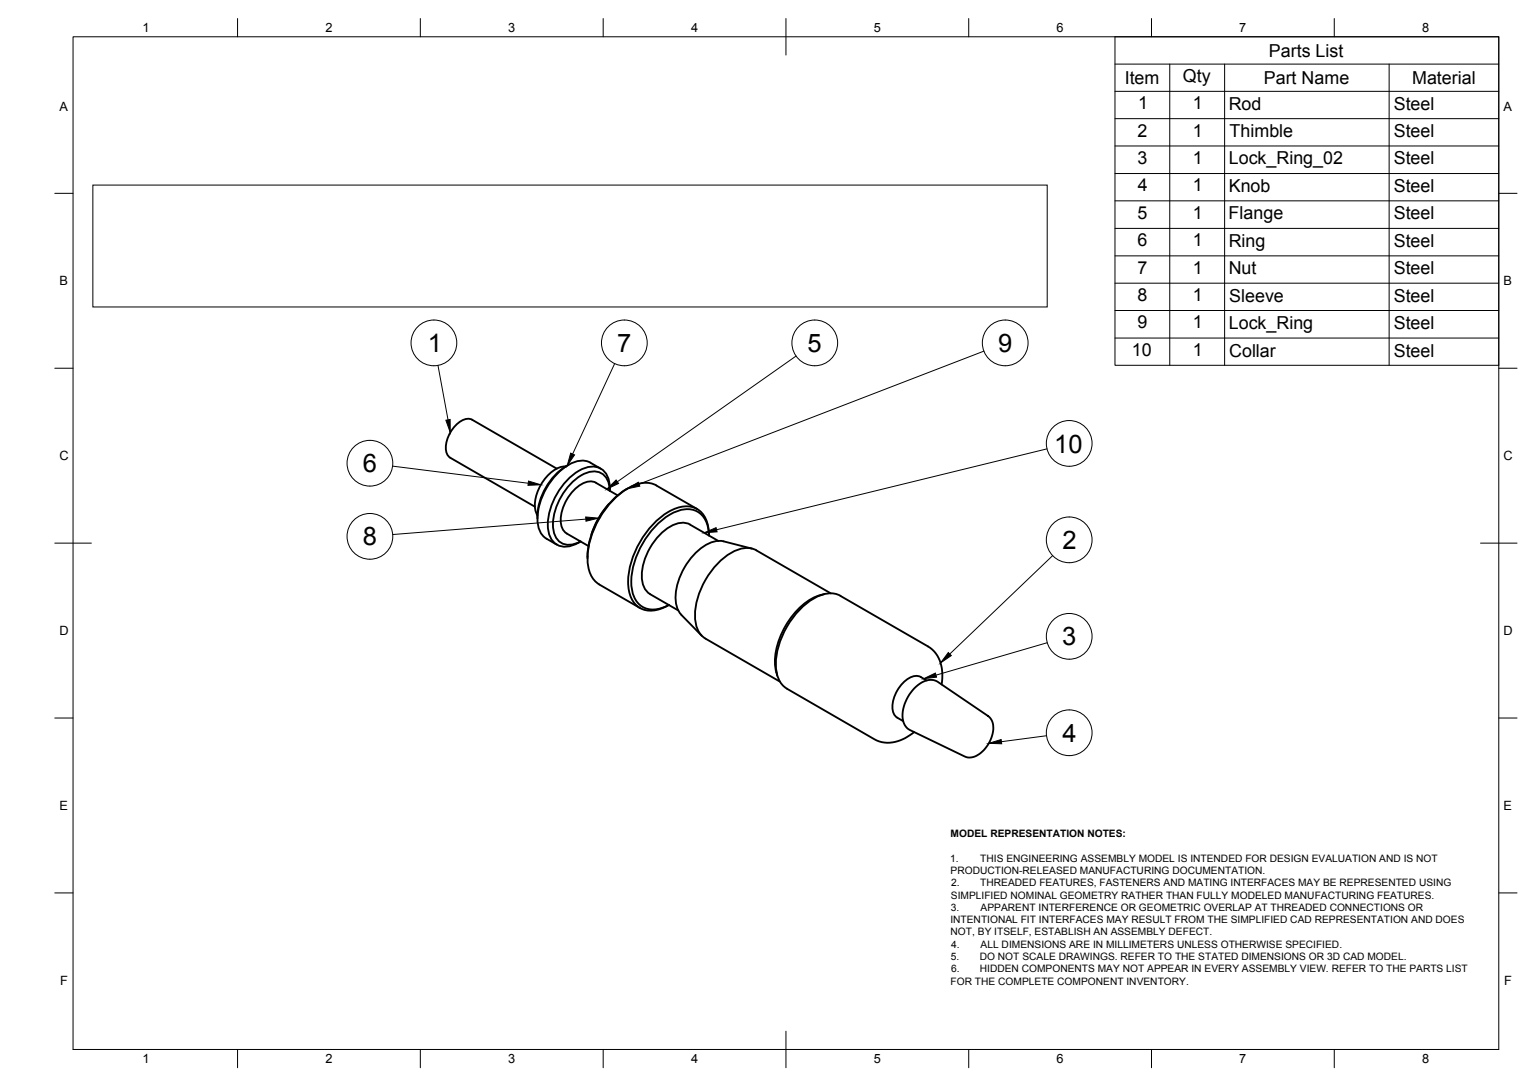
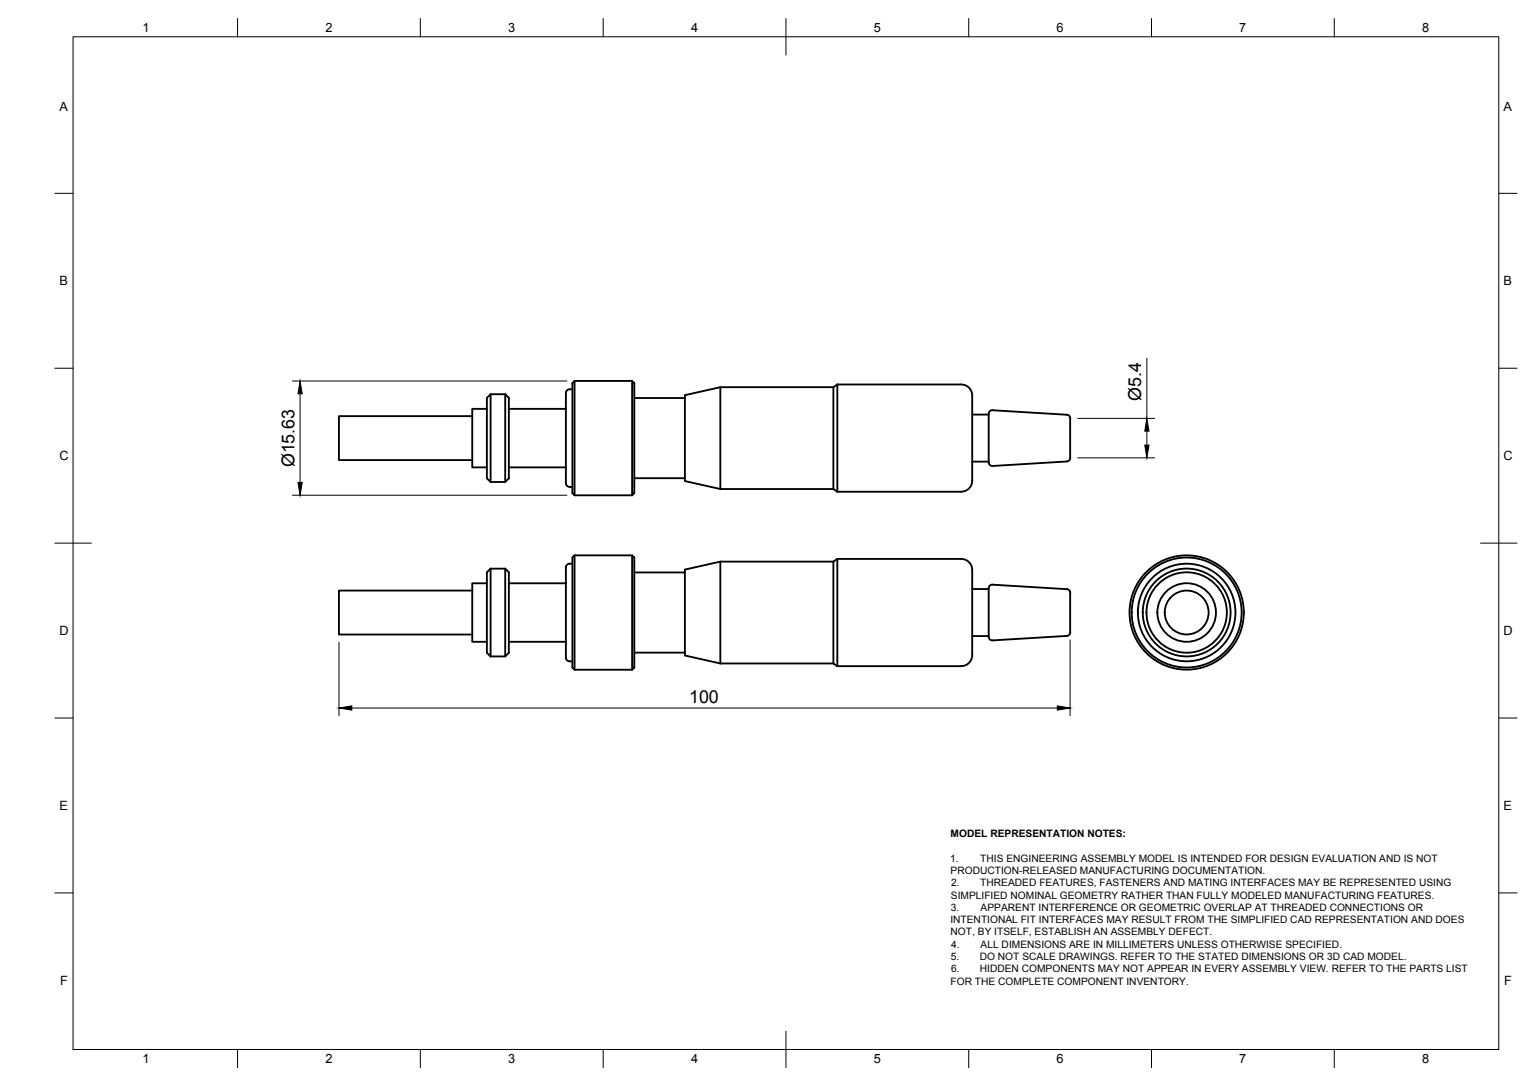
ISO-10303-21;
HEADER;
/* Generated by software containing ST-Developer
 * from STEP Tools, Inc. (www.steptools.com) 
 */

FILE_DESCRIPTION(
/* description */ (''),
/* implementation_level */ '2;1');

FILE_NAME(
/* name */ 'BR-156',
/* time_stamp */ '2026-10-05T01:33:24-07:00',
/* author */ (''),
/* organization */ (''),
/* preprocessor_version */ 'ST-DEVELOPER v20.2',
/* originating_system */ 'Autodesk Translation Framework v15.15.0.0',
/* authorisation */ '');

FILE_SCHEMA (('AUTOMOTIVE_DESIGN { 1 0 10303 214 3 1 1 }'));
ENDSEC;

DATA;
#10=MECHANICAL_DESIGN_GEOMETRIC_PRESENTATION_REPRESENTATION('',(#82,#83,
#84,#85,#86,#87,#88,#89,#90,#91),#1128);
#11=ITEM_DEFINED_TRANSFORMATION($,$,#643,#731);
#12=ITEM_DEFINED_TRANSFORMATION($,$,#649,#732);
#13=ITEM_DEFINED_TRANSFORMATION($,$,#664,#733);
#14=ITEM_DEFINED_TRANSFORMATION($,$,#670,#734);
#15=ITEM_DEFINED_TRANSFORMATION($,$,#682,#735);
#16=ITEM_DEFINED_TRANSFORMATION($,$,#688,#736);
#17=ITEM_DEFINED_TRANSFORMATION($,$,#694,#737);
#18=ITEM_DEFINED_TRANSFORMATION($,$,#704,#738);
#19=ITEM_DEFINED_TRANSFORMATION($,$,#713,#739);
#20=ITEM_DEFINED_TRANSFORMATION($,$,#725,#740);
#21=(
REPRESENTATION_RELATIONSHIP($,$,#1166,#1165)
REPRESENTATION_RELATIONSHIP_WITH_TRANSFORMATION(#11)
SHAPE_REPRESENTATION_RELATIONSHIP()
);
#22=(
REPRESENTATION_RELATIONSHIP($,$,#1167,#1165)
REPRESENTATION_RELATIONSHIP_WITH_TRANSFORMATION(#12)
SHAPE_REPRESENTATION_RELATIONSHIP()
);
#23=(
REPRESENTATION_RELATIONSHIP($,$,#1168,#1165)
REPRESENTATION_RELATIONSHIP_WITH_TRANSFORMATION(#13)
SHAPE_REPRESENTATION_RELATIONSHIP()
);
#24=(
REPRESENTATION_RELATIONSHIP($,$,#1169,#1165)
REPRESENTATION_RELATIONSHIP_WITH_TRANSFORMATION(#14)
SHAPE_REPRESENTATION_RELATIONSHIP()
);
#25=(
REPRESENTATION_RELATIONSHIP($,$,#1170,#1165)
REPRESENTATION_RELATIONSHIP_WITH_TRANSFORMATION(#15)
SHAPE_REPRESENTATION_RELATIONSHIP()
);
#26=(
REPRESENTATION_RELATIONSHIP($,$,#1171,#1165)
REPRESENTATION_RELATIONSHIP_WITH_TRANSFORMATION(#16)
SHAPE_REPRESENTATION_RELATIONSHIP()
);
#27=(
REPRESENTATION_RELATIONSHIP($,$,#1172,#1165)
REPRESENTATION_RELATIONSHIP_WITH_TRANSFORMATION(#17)
SHAPE_REPRESENTATION_RELATIONSHIP()
);
#28=(
REPRESENTATION_RELATIONSHIP($,$,#1173,#1165)
REPRESENTATION_RELATIONSHIP_WITH_TRANSFORMATION(#18)
SHAPE_REPRESENTATION_RELATIONSHIP()
);
#29=(
REPRESENTATION_RELATIONSHIP($,$,#1174,#1165)
REPRESENTATION_RELATIONSHIP_WITH_TRANSFORMATION(#19)
SHAPE_REPRESENTATION_RELATIONSHIP()
);
#30=(
REPRESENTATION_RELATIONSHIP($,$,#1175,#1165)
REPRESENTATION_RELATIONSHIP_WITH_TRANSFORMATION(#20)
SHAPE_REPRESENTATION_RELATIONSHIP()
);
#31=CONTEXT_DEPENDENT_SHAPE_REPRESENTATION(#21,#1155);
#32=CONTEXT_DEPENDENT_SHAPE_REPRESENTATION(#22,#1156);
#33=CONTEXT_DEPENDENT_SHAPE_REPRESENTATION(#23,#1157);
#34=CONTEXT_DEPENDENT_SHAPE_REPRESENTATION(#24,#1158);
#35=CONTEXT_DEPENDENT_SHAPE_REPRESENTATION(#25,#1159);
#36=CONTEXT_DEPENDENT_SHAPE_REPRESENTATION(#26,#1160);
#37=CONTEXT_DEPENDENT_SHAPE_REPRESENTATION(#27,#1161);
#38=CONTEXT_DEPENDENT_SHAPE_REPRESENTATION(#28,#1162);
#39=CONTEXT_DEPENDENT_SHAPE_REPRESENTATION(#29,#1163);
#40=CONTEXT_DEPENDENT_SHAPE_REPRESENTATION(#30,#1164);
#41=NEXT_ASSEMBLY_USAGE_OCCURRENCE('Rod:1','Rod:1','Rod:1',#1177,#1178,
'Rod:1');
#42=NEXT_ASSEMBLY_USAGE_OCCURRENCE('Thimble:1','Thimble:1','Thimble:1',
#1177,#1179,'Thimble:1');
#43=NEXT_ASSEMBLY_USAGE_OCCURRENCE('Lock_Ring_02:1','Lock_Ring_02:1',
'Lock_Ring_02:1',#1177,#1180,'Lock_Ring_02:1');
#44=NEXT_ASSEMBLY_USAGE_OCCURRENCE('Knob:1','Knob:1','Knob:1',#1177,#1181,
'Knob:1');
#45=NEXT_ASSEMBLY_USAGE_OCCURRENCE('Flange:1','Flange:1','Flange:1',#1177,
#1182,'Flange:1');
#46=NEXT_ASSEMBLY_USAGE_OCCURRENCE('Ring:1','Ring:1','Ring:1',#1177,#1183,
'Ring:1');
#47=NEXT_ASSEMBLY_USAGE_OCCURRENCE('Nut:1','Nut:1','Nut:1',#1177,#1184,
'Nut:1');
#48=NEXT_ASSEMBLY_USAGE_OCCURRENCE('Sleeve:1','Sleeve:1','Sleeve:1',#1177,
#1185,'Sleeve:1');
#49=NEXT_ASSEMBLY_USAGE_OCCURRENCE('Lock_Ring:1','Lock_Ring:1',
'Lock_Ring:1',#1177,#1186,'Lock_Ring:1');
#50=NEXT_ASSEMBLY_USAGE_OCCURRENCE('Collar:1','Collar:1','Collar:1',#1177,
#1187,'Collar:1');
#51=TOROIDAL_SURFACE('',#659,5.82799886529799,1.5);
#52=TOROIDAL_SURFACE('',#673,3.3075988470339,0.49999999999999);
#53=TOROIDAL_SURFACE('',#678,2.69979677377649,0.500000000000025);
#54=TOROIDAL_SURFACE('',#709,6.1693331034204,0.499999999999997);
#55=CONICAL_SURFACE('',#650,6.41661225190487,0.22222982204112);
#56=CONICAL_SURFACE('',#655,7.14605510547863,0.59398290857058);
#57=CONICAL_SURFACE('',#676,3.50280261490539,0.0598485673150425);
#58=CONICAL_SURFACE('',#695,5.75,0.785398163397451);
#59=CONICAL_SURFACE('',#700,5.75,0.785398163397451);
#60=CONICAL_SURFACE('',#714,7.66499874644978,0.785398163397445);
#61=CONICAL_SURFACE('',#722,7.66499874644978,0.785398163397452);
#62=SHAPE_REPRESENTATION_RELATIONSHIP('SRR','None',#1166,#72);
#63=SHAPE_REPRESENTATION_RELATIONSHIP('SRR','None',#1167,#73);
#64=SHAPE_REPRESENTATION_RELATIONSHIP('SRR','None',#1168,#74);
#65=SHAPE_REPRESENTATION_RELATIONSHIP('SRR','None',#1169,#75);
#66=SHAPE_REPRESENTATION_RELATIONSHIP('SRR','None',#1170,#76);
#67=SHAPE_REPRESENTATION_RELATIONSHIP('SRR','None',#1171,#77);
#68=SHAPE_REPRESENTATION_RELATIONSHIP('SRR','None',#1172,#78);
#69=SHAPE_REPRESENTATION_RELATIONSHIP('SRR','None',#1173,#79);
#70=SHAPE_REPRESENTATION_RELATIONSHIP('SRR','None',#1174,#80);
#71=SHAPE_REPRESENTATION_RELATIONSHIP('SRR','None',#1175,#81);
#72=ADVANCED_BREP_SHAPE_REPRESENTATION('',(#92),#1118);
#73=ADVANCED_BREP_SHAPE_REPRESENTATION('',(#93),#1119);
#74=ADVANCED_BREP_SHAPE_REPRESENTATION('',(#94),#1120);
#75=ADVANCED_BREP_SHAPE_REPRESENTATION('',(#95),#1121);
#76=ADVANCED_BREP_SHAPE_REPRESENTATION('',(#96),#1122);
#77=ADVANCED_BREP_SHAPE_REPRESENTATION('',(#97),#1123);
#78=ADVANCED_BREP_SHAPE_REPRESENTATION('',(#98),#1124);
#79=ADVANCED_BREP_SHAPE_REPRESENTATION('',(#99),#1125);
#80=ADVANCED_BREP_SHAPE_REPRESENTATION('',(#100),#1126);
#81=ADVANCED_BREP_SHAPE_REPRESENTATION('',(#101),#1127);
#82=STYLED_ITEM('',(#1225),#92);
#83=STYLED_ITEM('',(#1225),#93);
#84=STYLED_ITEM('',(#1226),#94);
#85=STYLED_ITEM('',(#1225),#95);
#86=STYLED_ITEM('',(#1227),#96);
#87=STYLED_ITEM('',(#1227),#97);
#88=STYLED_ITEM('',(#1227),#98);
#89=STYLED_ITEM('',(#1227),#99);
#90=STYLED_ITEM('',(#1225),#100);
#91=STYLED_ITEM('',(#1225),#101);
#92=MANIFOLD_SOLID_BREP('Body1',#521);
#93=MANIFOLD_SOLID_BREP('Body1',#522);
#94=MANIFOLD_SOLID_BREP('Body1',#523);
#95=MANIFOLD_SOLID_BREP('Body1',#524);
#96=MANIFOLD_SOLID_BREP('Body1',#525);
#97=MANIFOLD_SOLID_BREP('Body1',#526);
#98=MANIFOLD_SOLID_BREP('Body1',#527);
#99=MANIFOLD_SOLID_BREP('Body1',#528);
#100=MANIFOLD_SOLID_BREP('Body1',#529);
#101=MANIFOLD_SOLID_BREP('Body1',#530);
#102=LINE('',#964,#119);
#103=LINE('',#971,#120);
#104=LINE('',#976,#121);
#105=LINE('',#980,#122);
#106=LINE('',#984,#123);
#107=LINE('',#996,#124);
#108=LINE('',#1010,#125);
#109=LINE('',#1025,#126);
#110=LINE('',#1034,#127);
#111=LINE('',#1040,#128);
#112=LINE('',#1045,#129);
#113=LINE('',#1048,#130);
#114=LINE('',#1064,#131);
#115=LINE('',#1071,#132);
#116=LINE('',#1076,#133);
#117=LINE('',#1083,#134);
#118=LINE('',#1094,#135);
#119=VECTOR('',#753,3.);
#120=VECTOR('',#762,6.41661225190487);
#121=VECTOR('',#769,6.96411134565927);
#122=VECTOR('',#774,7.14605510547863);
#123=VECTOR('',#779,7.327998865298);
#124=VECTOR('',#796,3.21047290937838);
#125=VECTOR('',#817,3.50280261490539);
#126=VECTOR('',#840,4.);
#127=VECTOR('',#853,4.);
#128=VECTOR('',#860,5.75);
#129=VECTOR('',#867,6.);
#130=VECTOR('',#870,5.75);
#131=VECTOR('',#895,6.66933310342039);
#132=VECTOR('',#902,7.66499874644978);
#133=VECTOR('',#909,7.81499874644978);
#134=VECTOR('',#918,7.66499874644978);
#135=VECTOR('',#935,5.48257260644808);
#136=CYLINDRICAL_SURFACE('',#646,3.);
#137=CYLINDRICAL_SURFACE('',#653,6.96411134565927);
#138=CYLINDRICAL_SURFACE('',#657,7.327998865298);
#139=CYLINDRICAL_SURFACE('',#665,3.21047290937838);
#140=CYLINDRICAL_SURFACE('',#687,4.);
#141=CYLINDRICAL_SURFACE('',#693,4.);
#142=CYLINDRICAL_SURFACE('',#698,6.);
#143=CYLINDRICAL_SURFACE('',#712,6.66933310342039);
#144=CYLINDRICAL_SURFACE('',#718,7.81499874644978);
#145=CYLINDRICAL_SURFACE('',#730,5.48257260644808);
#146=FACE_OUTER_BOUND('',#187,.T.);
#147=FACE_OUTER_BOUND('',#188,.T.);
#148=FACE_OUTER_BOUND('',#189,.T.);
#149=FACE_OUTER_BOUND('',#190,.T.);
#150=FACE_OUTER_BOUND('',#191,.T.);
#151=FACE_OUTER_BOUND('',#192,.T.);
#152=FACE_OUTER_BOUND('',#193,.T.);
#153=FACE_OUTER_BOUND('',#194,.T.);
#154=FACE_OUTER_BOUND('',#195,.T.);
#155=FACE_OUTER_BOUND('',#196,.T.);
#156=FACE_OUTER_BOUND('',#197,.T.);
#157=FACE_OUTER_BOUND('',#198,.T.);
#158=FACE_OUTER_BOUND('',#199,.T.);
#159=FACE_OUTER_BOUND('',#200,.T.);
#160=FACE_OUTER_BOUND('',#201,.T.);
#161=FACE_OUTER_BOUND('',#202,.T.);
#162=FACE_OUTER_BOUND('',#203,.T.);
#163=FACE_OUTER_BOUND('',#204,.T.);
#164=FACE_OUTER_BOUND('',#205,.T.);
#165=FACE_OUTER_BOUND('',#206,.T.);
#166=FACE_OUTER_BOUND('',#207,.T.);
#167=FACE_OUTER_BOUND('',#208,.T.);
#168=FACE_OUTER_BOUND('',#209,.T.);
#169=FACE_OUTER_BOUND('',#210,.T.);
#170=FACE_OUTER_BOUND('',#211,.T.);
#171=FACE_OUTER_BOUND('',#212,.T.);
#172=FACE_OUTER_BOUND('',#213,.T.);
#173=FACE_OUTER_BOUND('',#214,.T.);
#174=FACE_OUTER_BOUND('',#215,.T.);
#175=FACE_OUTER_BOUND('',#216,.T.);
#176=FACE_OUTER_BOUND('',#217,.T.);
#177=FACE_OUTER_BOUND('',#218,.T.);
#178=FACE_OUTER_BOUND('',#219,.T.);
#179=FACE_OUTER_BOUND('',#220,.T.);
#180=FACE_OUTER_BOUND('',#221,.T.);
#181=FACE_OUTER_BOUND('',#222,.T.);
#182=FACE_OUTER_BOUND('',#223,.T.);
#183=FACE_OUTER_BOUND('',#224,.T.);
#184=FACE_OUTER_BOUND('',#225,.T.);
#185=FACE_OUTER_BOUND('',#226,.T.);
#186=FACE_OUTER_BOUND('',#227,.T.);
#187=EDGE_LOOP('',(#352));
#188=EDGE_LOOP('',(#353,#354,#355,#356));
#189=EDGE_LOOP('',(#357));
#190=EDGE_LOOP('',(#358,#359,#360,#361));
#191=EDGE_LOOP('',(#362,#363,#364,#365));
#192=EDGE_LOOP('',(#366,#367,#368,#369));
#193=EDGE_LOOP('',(#370,#371,#372,#373));
#194=EDGE_LOOP('',(#374,#375,#376,#377));
#195=EDGE_LOOP('',(#378));
#196=EDGE_LOOP('',(#379));
#197=EDGE_LOOP('',(#380,#381,#382,#383));
#198=EDGE_LOOP('',(#384));
#199=EDGE_LOOP('',(#385));
#200=EDGE_LOOP('',(#386));
#201=EDGE_LOOP('',(#387,#388,#389,#390));
#202=EDGE_LOOP('',(#391,#392,#393,#394));
#203=EDGE_LOOP('',(#395,#396,#397,#398));
#204=EDGE_LOOP('',(#399));
#205=EDGE_LOOP('',(#400));
#206=EDGE_LOOP('',(#401));
#207=EDGE_LOOP('',(#402,#403,#404,#405));
#208=EDGE_LOOP('',(#406));
#209=EDGE_LOOP('',(#407));
#210=EDGE_LOOP('',(#408,#409,#410,#411));
#211=EDGE_LOOP('',(#412,#413,#414,#415));
#212=EDGE_LOOP('',(#416,#417,#418,#419));
#213=EDGE_LOOP('',(#420,#421,#422,#423));
#214=EDGE_LOOP('',(#424));
#215=EDGE_LOOP('',(#425));
#216=EDGE_LOOP('',(#426));
#217=EDGE_LOOP('',(#427));
#218=EDGE_LOOP('',(#428,#429,#430,#431));
#219=EDGE_LOOP('',(#432,#433,#434,#435));
#220=EDGE_LOOP('',(#436,#437,#438,#439,#440));
#221=EDGE_LOOP('',(#441,#442,#443,#444,#445,#446));
#222=EDGE_LOOP('',(#447));
#223=EDGE_LOOP('',(#448,#449,#450,#451,#452));
#224=EDGE_LOOP('',(#453));
#225=EDGE_LOOP('',(#454));
#226=EDGE_LOOP('',(#455));
#227=EDGE_LOOP('',(#456,#457,#458,#459));
#228=CIRCLE('',#645,3.);
#229=CIRCLE('',#647,3.);
#230=CIRCLE('',#651,6.96411134565927);
#231=CIRCLE('',#652,5.86911315815046);
#232=CIRCLE('',#654,6.96411134565926);
#233=CIRCLE('',#656,7.327998865298);
#234=CIRCLE('',#658,7.327998865298);
#235=CIRCLE('',#660,5.827998865298);
#236=CIRCLE('',#661,1.5);
#237=CIRCLE('',#666,3.21047290937838);
#238=CIRCLE('',#667,3.21047290937838);
#239=CIRCLE('',#672,3.3075988470339);
#240=CIRCLE('',#674,3.80670365153407);
#241=CIRCLE('',#675,0.49999999999999);
#242=CIRCLE('',#677,3.1989015782767);
#243=CIRCLE('',#679,2.69979677377651);
#244=CIRCLE('',#680,0.500000000000025);
#245=CIRCLE('',#684,4.);
#246=CIRCLE('',#686,4.);
#247=CIRCLE('',#690,4.);
#248=CIRCLE('',#692,4.);
#249=CIRCLE('',#696,6.);
#250=CIRCLE('',#697,5.5);
#251=CIRCLE('',#699,6.);
#252=CIRCLE('',#701,5.5);
#253=CIRCLE('',#706,6.66933310342039);
#254=CIRCLE('',#708,6.16933310342039);
#255=CIRCLE('',#710,6.66933310342039);
#256=CIRCLE('',#711,0.499999999999997);
#257=CIRCLE('',#715,7.81499874644978);
#258=CIRCLE('',#716,7.51499874644978);
#259=CIRCLE('',#717,7.81499874644978);
#260=CIRCLE('',#719,7.81499874644978);
#261=CIRCLE('',#720,7.81499874644978);
#262=CIRCLE('',#723,7.51499874644978);
#263=CIRCLE('',#727,5.48257260644808);
#264=CIRCLE('',#729,5.48257260644808);
#265=VERTEX_POINT('',#959);
#266=VERTEX_POINT('',#962);
#267=VERTEX_POINT('',#968);
#268=VERTEX_POINT('',#970);
#269=VERTEX_POINT('',#974);
#270=VERTEX_POINT('',#978);
#271=VERTEX_POINT('',#982);
#272=VERTEX_POINT('',#986);
#273=VERTEX_POINT('',#993);
#274=VERTEX_POINT('',#995);
#275=VERTEX_POINT('',#1002);
#276=VERTEX_POINT('',#1005);
#277=VERTEX_POINT('',#1009);
#278=VERTEX_POINT('',#1013);
#279=VERTEX_POINT('',#1019);
#280=VERTEX_POINT('',#1022);
#281=VERTEX_POINT('',#1028);
#282=VERTEX_POINT('',#1031);
#283=VERTEX_POINT('',#1037);
#284=VERTEX_POINT('',#1039);
#285=VERTEX_POINT('',#1043);
#286=VERTEX_POINT('',#1047);
#287=VERTEX_POINT('',#1054);
#288=VERTEX_POINT('',#1057);
#289=VERTEX_POINT('',#1060);
#290=VERTEX_POINT('',#1067);
#291=VERTEX_POINT('',#1068);
#292=VERTEX_POINT('',#1070);
#293=VERTEX_POINT('',#1075);
#294=VERTEX_POINT('',#1077);
#295=VERTEX_POINT('',#1082);
#296=VERTEX_POINT('',#1088);
#297=VERTEX_POINT('',#1091);
#298=EDGE_CURVE('',#265,#265,#228,.T.);
#299=EDGE_CURVE('',#266,#266,#229,.T.);
#300=EDGE_CURVE('',#266,#265,#102,.T.);
#301=EDGE_CURVE('',#267,#267,#230,.T.);
#302=EDGE_CURVE('',#267,#268,#103,.T.);
#303=EDGE_CURVE('',#268,#268,#231,.T.);
#304=EDGE_CURVE('',#269,#269,#232,.T.);
#305=EDGE_CURVE('',#269,#267,#104,.T.);
#306=EDGE_CURVE('',#270,#270,#233,.T.);
#307=EDGE_CURVE('',#270,#269,#105,.T.);
#308=EDGE_CURVE('',#271,#271,#234,.T.);
#309=EDGE_CURVE('',#271,#270,#106,.T.);
#310=EDGE_CURVE('',#272,#272,#235,.T.);
#311=EDGE_CURVE('',#272,#271,#236,.T.);
#312=EDGE_CURVE('',#273,#273,#237,.T.);
#313=EDGE_CURVE('',#273,#274,#107,.T.);
#314=EDGE_CURVE('',#274,#274,#238,.T.);
#315=EDGE_CURVE('',#275,#275,#239,.T.);
#316=EDGE_CURVE('',#276,#276,#240,.T.);
#317=EDGE_CURVE('',#276,#275,#241,.T.);
#318=EDGE_CURVE('',#276,#277,#108,.T.);
#319=EDGE_CURVE('',#277,#277,#242,.T.);
#320=EDGE_CURVE('',#278,#278,#243,.T.);
#321=EDGE_CURVE('',#278,#277,#244,.T.);
#322=EDGE_CURVE('',#279,#279,#245,.T.);
#323=EDGE_CURVE('',#280,#280,#246,.T.);
#324=EDGE_CURVE('',#279,#280,#109,.T.);
#325=EDGE_CURVE('',#281,#281,#247,.T.);
#326=EDGE_CURVE('',#282,#282,#248,.T.);
#327=EDGE_CURVE('',#281,#282,#110,.T.);
#328=EDGE_CURVE('',#283,#283,#249,.T.);
#329=EDGE_CURVE('',#283,#284,#111,.T.);
#330=EDGE_CURVE('',#284,#284,#250,.T.);
#331=EDGE_CURVE('',#285,#285,#251,.T.);
#332=EDGE_CURVE('',#285,#283,#112,.T.);
#333=EDGE_CURVE('',#285,#286,#113,.T.);
#334=EDGE_CURVE('',#286,#286,#252,.T.);
#335=EDGE_CURVE('',#287,#287,#253,.T.);
#336=EDGE_CURVE('',#288,#288,#254,.T.);
#337=EDGE_CURVE('',#289,#289,#255,.T.);
#338=EDGE_CURVE('',#289,#288,#256,.T.);
#339=EDGE_CURVE('',#287,#289,#114,.T.);
#340=EDGE_CURVE('',#290,#291,#257,.T.);
#341=EDGE_CURVE('',#291,#292,#115,.T.);
#342=EDGE_CURVE('',#292,#292,#258,.T.);
#343=EDGE_CURVE('',#291,#290,#259,.T.);
#344=EDGE_CURVE('',#290,#293,#116,.T.);
#345=EDGE_CURVE('',#294,#293,#260,.T.);
#346=EDGE_CURVE('',#293,#294,#261,.T.);
#347=EDGE_CURVE('',#294,#295,#117,.T.);
#348=EDGE_CURVE('',#295,#295,#262,.T.);
#349=EDGE_CURVE('',#296,#296,#263,.T.);
#350=EDGE_CURVE('',#297,#297,#264,.T.);
#351=EDGE_CURVE('',#296,#297,#118,.T.);
#352=ORIENTED_EDGE('',*,*,#298,.F.);
#353=ORIENTED_EDGE('',*,*,#299,.F.);
#354=ORIENTED_EDGE('',*,*,#300,.T.);
#355=ORIENTED_EDGE('',*,*,#298,.T.);
#356=ORIENTED_EDGE('',*,*,#300,.F.);
#357=ORIENTED_EDGE('',*,*,#299,.T.);
#358=ORIENTED_EDGE('',*,*,#301,.F.);
#359=ORIENTED_EDGE('',*,*,#302,.T.);
#360=ORIENTED_EDGE('',*,*,#303,.T.);
#361=ORIENTED_EDGE('',*,*,#302,.F.);
#362=ORIENTED_EDGE('',*,*,#304,.F.);
#363=ORIENTED_EDGE('',*,*,#305,.T.);
#364=ORIENTED_EDGE('',*,*,#301,.T.);
#365=ORIENTED_EDGE('',*,*,#305,.F.);
#366=ORIENTED_EDGE('',*,*,#306,.F.);
#367=ORIENTED_EDGE('',*,*,#307,.T.);
#368=ORIENTED_EDGE('',*,*,#304,.T.);
#369=ORIENTED_EDGE('',*,*,#307,.F.);
#370=ORIENTED_EDGE('',*,*,#308,.F.);
#371=ORIENTED_EDGE('',*,*,#309,.T.);
#372=ORIENTED_EDGE('',*,*,#306,.T.);
#373=ORIENTED_EDGE('',*,*,#309,.F.);
#374=ORIENTED_EDGE('',*,*,#310,.F.);
#375=ORIENTED_EDGE('',*,*,#311,.T.);
#376=ORIENTED_EDGE('',*,*,#308,.T.);
#377=ORIENTED_EDGE('',*,*,#311,.F.);
#378=ORIENTED_EDGE('',*,*,#310,.T.);
#379=ORIENTED_EDGE('',*,*,#303,.F.);
#380=ORIENTED_EDGE('',*,*,#312,.F.);
#381=ORIENTED_EDGE('',*,*,#313,.T.);
#382=ORIENTED_EDGE('',*,*,#314,.T.);
#383=ORIENTED_EDGE('',*,*,#313,.F.);
#384=ORIENTED_EDGE('',*,*,#312,.T.);
#385=ORIENTED_EDGE('',*,*,#314,.F.);
#386=ORIENTED_EDGE('',*,*,#315,.F.);
#387=ORIENTED_EDGE('',*,*,#316,.F.);
#388=ORIENTED_EDGE('',*,*,#317,.T.);
#389=ORIENTED_EDGE('',*,*,#315,.T.);
#390=ORIENTED_EDGE('',*,*,#317,.F.);
#391=ORIENTED_EDGE('',*,*,#316,.T.);
#392=ORIENTED_EDGE('',*,*,#318,.T.);
#393=ORIENTED_EDGE('',*,*,#319,.F.);
#394=ORIENTED_EDGE('',*,*,#318,.F.);
#395=ORIENTED_EDGE('',*,*,#320,.F.);
#396=ORIENTED_EDGE('',*,*,#321,.T.);
#397=ORIENTED_EDGE('',*,*,#319,.T.);
#398=ORIENTED_EDGE('',*,*,#321,.F.);
#399=ORIENTED_EDGE('',*,*,#320,.T.);
#400=ORIENTED_EDGE('',*,*,#322,.T.);
#401=ORIENTED_EDGE('',*,*,#323,.F.);
#402=ORIENTED_EDGE('',*,*,#322,.F.);
#403=ORIENTED_EDGE('',*,*,#324,.T.);
#404=ORIENTED_EDGE('',*,*,#323,.T.);
#405=ORIENTED_EDGE('',*,*,#324,.F.);
#406=ORIENTED_EDGE('',*,*,#325,.T.);
#407=ORIENTED_EDGE('',*,*,#326,.F.);
#408=ORIENTED_EDGE('',*,*,#325,.F.);
#409=ORIENTED_EDGE('',*,*,#327,.T.);
#410=ORIENTED_EDGE('',*,*,#326,.T.);
#411=ORIENTED_EDGE('',*,*,#327,.F.);
#412=ORIENTED_EDGE('',*,*,#328,.F.);
#413=ORIENTED_EDGE('',*,*,#329,.T.);
#414=ORIENTED_EDGE('',*,*,#330,.T.);
#415=ORIENTED_EDGE('',*,*,#329,.F.);
#416=ORIENTED_EDGE('',*,*,#331,.F.);
#417=ORIENTED_EDGE('',*,*,#332,.T.);
#418=ORIENTED_EDGE('',*,*,#328,.T.);
#419=ORIENTED_EDGE('',*,*,#332,.F.);
#420=ORIENTED_EDGE('',*,*,#331,.T.);
#421=ORIENTED_EDGE('',*,*,#333,.T.);
#422=ORIENTED_EDGE('',*,*,#334,.F.);
#423=ORIENTED_EDGE('',*,*,#333,.F.);
#424=ORIENTED_EDGE('',*,*,#334,.T.);
#425=ORIENTED_EDGE('',*,*,#330,.F.);
#426=ORIENTED_EDGE('',*,*,#335,.T.);
#427=ORIENTED_EDGE('',*,*,#336,.F.);
#428=ORIENTED_EDGE('',*,*,#337,.F.);
#429=ORIENTED_EDGE('',*,*,#338,.T.);
#430=ORIENTED_EDGE('',*,*,#336,.T.);
#431=ORIENTED_EDGE('',*,*,#338,.F.);
#432=ORIENTED_EDGE('',*,*,#335,.F.);
#433=ORIENTED_EDGE('',*,*,#339,.T.);
#434=ORIENTED_EDGE('',*,*,#337,.T.);
#435=ORIENTED_EDGE('',*,*,#339,.F.);
#436=ORIENTED_EDGE('',*,*,#340,.T.);
#437=ORIENTED_EDGE('',*,*,#341,.T.);
#438=ORIENTED_EDGE('',*,*,#342,.T.);
#439=ORIENTED_EDGE('',*,*,#341,.F.);
#440=ORIENTED_EDGE('',*,*,#343,.T.);
#441=ORIENTED_EDGE('',*,*,#340,.F.);
#442=ORIENTED_EDGE('',*,*,#344,.T.);
#443=ORIENTED_EDGE('',*,*,#345,.F.);
#444=ORIENTED_EDGE('',*,*,#346,.F.);
#445=ORIENTED_EDGE('',*,*,#344,.F.);
#446=ORIENTED_EDGE('',*,*,#343,.F.);
#447=ORIENTED_EDGE('',*,*,#342,.F.);
#448=ORIENTED_EDGE('',*,*,#345,.T.);
#449=ORIENTED_EDGE('',*,*,#346,.T.);
#450=ORIENTED_EDGE('',*,*,#347,.T.);
#451=ORIENTED_EDGE('',*,*,#348,.T.);
#452=ORIENTED_EDGE('',*,*,#347,.F.);
#453=ORIENTED_EDGE('',*,*,#348,.F.);
#454=ORIENTED_EDGE('',*,*,#349,.T.);
#455=ORIENTED_EDGE('',*,*,#350,.F.);
#456=ORIENTED_EDGE('',*,*,#349,.F.);
#457=ORIENTED_EDGE('',*,*,#351,.T.);
#458=ORIENTED_EDGE('',*,*,#350,.T.);
#459=ORIENTED_EDGE('',*,*,#351,.F.);
#460=PLANE('',#644);
#461=PLANE('',#648);
#462=PLANE('',#662);
#463=PLANE('',#663);
#464=PLANE('',#668);
#465=PLANE('',#669);
#466=PLANE('',#671);
#467=PLANE('',#681);
#468=PLANE('',#683);
#469=PLANE('',#685);
#470=PLANE('',#689);
#471=PLANE('',#691);
#472=PLANE('',#702);
#473=PLANE('',#703);
#474=PLANE('',#705);
#475=PLANE('',#707);
#476=PLANE('',#721);
#477=PLANE('',#724);
#478=PLANE('',#726);
#479=PLANE('',#728);
#480=ADVANCED_FACE('',(#146),#460,.T.);
#481=ADVANCED_FACE('',(#147),#136,.T.);
#482=ADVANCED_FACE('',(#148),#461,.T.);
#483=ADVANCED_FACE('',(#149),#55,.T.);
#484=ADVANCED_FACE('',(#150),#137,.T.);
#485=ADVANCED_FACE('',(#151),#56,.T.);
#486=ADVANCED_FACE('',(#152),#138,.T.);
#487=ADVANCED_FACE('',(#153),#51,.T.);
#488=ADVANCED_FACE('',(#154),#462,.T.);
#489=ADVANCED_FACE('',(#155),#463,.T.);
#490=ADVANCED_FACE('',(#156),#139,.T.);
#491=ADVANCED_FACE('',(#157),#464,.T.);
#492=ADVANCED_FACE('',(#158),#465,.T.);
#493=ADVANCED_FACE('',(#159),#466,.T.);
#494=ADVANCED_FACE('',(#160),#52,.T.);
#495=ADVANCED_FACE('',(#161),#57,.T.);
#496=ADVANCED_FACE('',(#162),#53,.T.);
#497=ADVANCED_FACE('',(#163),#467,.T.);
#498=ADVANCED_FACE('',(#164),#468,.T.);
#499=ADVANCED_FACE('',(#165),#469,.T.);
#500=ADVANCED_FACE('',(#166),#140,.T.);
#501=ADVANCED_FACE('',(#167),#470,.T.);
#502=ADVANCED_FACE('',(#168),#471,.T.);
#503=ADVANCED_FACE('',(#169),#141,.T.);
#504=ADVANCED_FACE('',(#170),#58,.T.);
#505=ADVANCED_FACE('',(#171),#142,.T.);
#506=ADVANCED_FACE('',(#172),#59,.T.);
#507=ADVANCED_FACE('',(#173),#472,.T.);
#508=ADVANCED_FACE('',(#174),#473,.T.);
#509=ADVANCED_FACE('',(#175),#474,.T.);
#510=ADVANCED_FACE('',(#176),#475,.T.);
#511=ADVANCED_FACE('',(#177),#54,.T.);
#512=ADVANCED_FACE('',(#178),#143,.T.);
#513=ADVANCED_FACE('',(#179),#60,.T.);
#514=ADVANCED_FACE('',(#180),#144,.T.);
#515=ADVANCED_FACE('',(#181),#476,.T.);
#516=ADVANCED_FACE('',(#182),#61,.T.);
#517=ADVANCED_FACE('',(#183),#477,.T.);
#518=ADVANCED_FACE('',(#184),#478,.T.);
#519=ADVANCED_FACE('',(#185),#479,.T.);
#520=ADVANCED_FACE('',(#186),#145,.T.);
#521=CLOSED_SHELL('',(#480,#481,#482));
#522=CLOSED_SHELL('',(#483,#484,#485,#486,#487,#488,#489));
#523=CLOSED_SHELL('',(#490,#491,#492));
#524=CLOSED_SHELL('',(#493,#494,#495,#496,#497));
#525=CLOSED_SHELL('',(#498,#499,#500));
#526=CLOSED_SHELL('',(#501,#502,#503));
#527=CLOSED_SHELL('',(#504,#505,#506,#507,#508));
#528=CLOSED_SHELL('',(#509,#510,#511,#512));
#529=CLOSED_SHELL('',(#513,#514,#515,#516,#517));
#530=CLOSED_SHELL('',(#518,#519,#520));
#531=DERIVED_UNIT_ELEMENT(#551,1.);
#532=DERIVED_UNIT_ELEMENT(#1130,-3.);
#533=DERIVED_UNIT_ELEMENT(#551,1.);
#534=DERIVED_UNIT_ELEMENT(#1130,-3.);
#535=DERIVED_UNIT_ELEMENT(#551,1.);
#536=DERIVED_UNIT_ELEMENT(#1130,-3.);
#537=DERIVED_UNIT_ELEMENT(#551,1.);
#538=DERIVED_UNIT_ELEMENT(#1130,-3.);
#539=DERIVED_UNIT_ELEMENT(#551,1.);
#540=DERIVED_UNIT_ELEMENT(#1130,-3.);
#541=DERIVED_UNIT_ELEMENT(#551,1.);
#542=DERIVED_UNIT_ELEMENT(#1130,-3.);
#543=DERIVED_UNIT_ELEMENT(#551,1.);
#544=DERIVED_UNIT_ELEMENT(#1130,-3.);
#545=DERIVED_UNIT_ELEMENT(#551,1.);
#546=DERIVED_UNIT_ELEMENT(#1130,-3.);
#547=DERIVED_UNIT_ELEMENT(#551,1.);
#548=DERIVED_UNIT_ELEMENT(#1130,-3.);
#549=DERIVED_UNIT_ELEMENT(#551,1.);
#550=DERIVED_UNIT_ELEMENT(#1130,-3.);
#551=(
MASS_UNIT()
NAMED_UNIT(*)
SI_UNIT(.KILO.,.GRAM.)
);
#552=DERIVED_UNIT((#531,#532));
#553=DERIVED_UNIT((#533,#534));
#554=DERIVED_UNIT((#535,#536));
#555=DERIVED_UNIT((#537,#538));
#556=DERIVED_UNIT((#539,#540));
#557=DERIVED_UNIT((#541,#542));
#558=DERIVED_UNIT((#543,#544));
#559=DERIVED_UNIT((#545,#546));
#560=DERIVED_UNIT((#547,#548));
#561=DERIVED_UNIT((#549,#550));
#562=MEASURE_REPRESENTATION_ITEM('density measure',
POSITIVE_RATIO_MEASURE(7850.),#552);
#563=MEASURE_REPRESENTATION_ITEM('density measure',
POSITIVE_RATIO_MEASURE(7850.),#553);
#564=MEASURE_REPRESENTATION_ITEM('density measure',
POSITIVE_RATIO_MEASURE(7850.),#554);
#565=MEASURE_REPRESENTATION_ITEM('density measure',
POSITIVE_RATIO_MEASURE(7850.),#555);
#566=MEASURE_REPRESENTATION_ITEM('density measure',
POSITIVE_RATIO_MEASURE(7850.),#556);
#567=MEASURE_REPRESENTATION_ITEM('density measure',
POSITIVE_RATIO_MEASURE(7850.),#557);
#568=MEASURE_REPRESENTATION_ITEM('density measure',
POSITIVE_RATIO_MEASURE(7850.),#558);
#569=MEASURE_REPRESENTATION_ITEM('density measure',
POSITIVE_RATIO_MEASURE(7850.),#559);
#570=MEASURE_REPRESENTATION_ITEM('density measure',
POSITIVE_RATIO_MEASURE(7850.),#560);
#571=MEASURE_REPRESENTATION_ITEM('density measure',
POSITIVE_RATIO_MEASURE(7850.),#561);
#572=PROPERTY_DEFINITION_REPRESENTATION(#622,#592);
#573=PROPERTY_DEFINITION_REPRESENTATION(#623,#593);
#574=PROPERTY_DEFINITION_REPRESENTATION(#624,#594);
#575=PROPERTY_DEFINITION_REPRESENTATION(#625,#595);
#576=PROPERTY_DEFINITION_REPRESENTATION(#626,#596);
#577=PROPERTY_DEFINITION_REPRESENTATION(#627,#597);
#578=PROPERTY_DEFINITION_REPRESENTATION(#628,#598);
#579=PROPERTY_DEFINITION_REPRESENTATION(#629,#599);
#580=PROPERTY_DEFINITION_REPRESENTATION(#630,#600);
#581=PROPERTY_DEFINITION_REPRESENTATION(#631,#601);
#582=PROPERTY_DEFINITION_REPRESENTATION(#632,#602);
#583=PROPERTY_DEFINITION_REPRESENTATION(#633,#603);
#584=PROPERTY_DEFINITION_REPRESENTATION(#634,#604);
#585=PROPERTY_DEFINITION_REPRESENTATION(#635,#605);
#586=PROPERTY_DEFINITION_REPRESENTATION(#636,#606);
#587=PROPERTY_DEFINITION_REPRESENTATION(#637,#607);
#588=PROPERTY_DEFINITION_REPRESENTATION(#638,#608);
#589=PROPERTY_DEFINITION_REPRESENTATION(#639,#609);
#590=PROPERTY_DEFINITION_REPRESENTATION(#640,#610);
#591=PROPERTY_DEFINITION_REPRESENTATION(#641,#611);
#592=REPRESENTATION('material name',(#612),#1118);
#593=REPRESENTATION('density',(#562),#1118);
#594=REPRESENTATION('material name',(#613),#1119);
#595=REPRESENTATION('density',(#563),#1119);
#596=REPRESENTATION('material name',(#614),#1120);
#597=REPRESENTATION('density',(#564),#1120);
#598=REPRESENTATION('material name',(#615),#1121);
#599=REPRESENTATION('density',(#565),#1121);
#600=REPRESENTATION('material name',(#616),#1122);
#601=REPRESENTATION('density',(#566),#1122);
#602=REPRESENTATION('material name',(#617),#1123);
#603=REPRESENTATION('density',(#567),#1123);
#604=REPRESENTATION('material name',(#618),#1124);
#605=REPRESENTATION('density',(#568),#1124);
#606=REPRESENTATION('material name',(#619),#1125);
#607=REPRESENTATION('density',(#569),#1125);
#608=REPRESENTATION('material name',(#620),#1126);
#609=REPRESENTATION('density',(#570),#1126);
#610=REPRESENTATION('material name',(#621),#1127);
#611=REPRESENTATION('density',(#571),#1127);
#612=DESCRIPTIVE_REPRESENTATION_ITEM('Steel','Steel');
#613=DESCRIPTIVE_REPRESENTATION_ITEM('Steel','Steel');
#614=DESCRIPTIVE_REPRESENTATION_ITEM('Steel','Steel');
#615=DESCRIPTIVE_REPRESENTATION_ITEM('Steel','Steel');
#616=DESCRIPTIVE_REPRESENTATION_ITEM('Steel','Steel');
#617=DESCRIPTIVE_REPRESENTATION_ITEM('Steel','Steel');
#618=DESCRIPTIVE_REPRESENTATION_ITEM('Steel','Steel');
#619=DESCRIPTIVE_REPRESENTATION_ITEM('Steel','Steel');
#620=DESCRIPTIVE_REPRESENTATION_ITEM('Steel','Steel');
#621=DESCRIPTIVE_REPRESENTATION_ITEM('Steel','Steel');
#622=PROPERTY_DEFINITION('material property','material name',#1178);
#623=PROPERTY_DEFINITION('material property','density of part',#1178);
#624=PROPERTY_DEFINITION('material property','material name',#1179);
#625=PROPERTY_DEFINITION('material property','density of part',#1179);
#626=PROPERTY_DEFINITION('material property','material name',#1180);
#627=PROPERTY_DEFINITION('material property','density of part',#1180);
#628=PROPERTY_DEFINITION('material property','material name',#1181);
#629=PROPERTY_DEFINITION('material property','density of part',#1181);
#630=PROPERTY_DEFINITION('material property','material name',#1182);
#631=PROPERTY_DEFINITION('material property','density of part',#1182);
#632=PROPERTY_DEFINITION('material property','material name',#1183);
#633=PROPERTY_DEFINITION('material property','density of part',#1183);
#634=PROPERTY_DEFINITION('material property','material name',#1184);
#635=PROPERTY_DEFINITION('material property','density of part',#1184);
#636=PROPERTY_DEFINITION('material property','material name',#1185);
#637=PROPERTY_DEFINITION('material property','density of part',#1185);
#638=PROPERTY_DEFINITION('material property','material name',#1186);
#639=PROPERTY_DEFINITION('material property','density of part',#1186);
#640=PROPERTY_DEFINITION('material property','material name',#1187);
#641=PROPERTY_DEFINITION('material property','density of part',#1187);
#642=AXIS2_PLACEMENT_3D('',#956,#741,#742);
#643=AXIS2_PLACEMENT_3D('',#957,#743,#744);
#644=AXIS2_PLACEMENT_3D('',#958,#745,#746);
#645=AXIS2_PLACEMENT_3D('',#960,#747,#748);
#646=AXIS2_PLACEMENT_3D('',#961,#749,#750);
#647=AXIS2_PLACEMENT_3D('',#963,#751,#752);
#648=AXIS2_PLACEMENT_3D('',#965,#754,#755);
#649=AXIS2_PLACEMENT_3D('',#966,#756,#757);
#650=AXIS2_PLACEMENT_3D('',#967,#758,#759);
#651=AXIS2_PLACEMENT_3D('',#969,#760,#761);
#652=AXIS2_PLACEMENT_3D('',#972,#763,#764);
#653=AXIS2_PLACEMENT_3D('',#973,#765,#766);
#654=AXIS2_PLACEMENT_3D('',#975,#767,#768);
#655=AXIS2_PLACEMENT_3D('',#977,#770,#771);
#656=AXIS2_PLACEMENT_3D('',#979,#772,#773);
#657=AXIS2_PLACEMENT_3D('',#981,#775,#776);
#658=AXIS2_PLACEMENT_3D('',#983,#777,#778);
#659=AXIS2_PLACEMENT_3D('',#985,#780,#781);
#660=AXIS2_PLACEMENT_3D('',#987,#782,#783);
#661=AXIS2_PLACEMENT_3D('',#988,#784,#785);
#662=AXIS2_PLACEMENT_3D('',#989,#786,#787);
#663=AXIS2_PLACEMENT_3D('',#990,#788,#789);
#664=AXIS2_PLACEMENT_3D('',#991,#790,#791);
#665=AXIS2_PLACEMENT_3D('',#992,#792,#793);
#666=AXIS2_PLACEMENT_3D('',#994,#794,#795);
#667=AXIS2_PLACEMENT_3D('',#997,#797,#798);
#668=AXIS2_PLACEMENT_3D('',#998,#799,#800);
#669=AXIS2_PLACEMENT_3D('',#999,#801,#802);
#670=AXIS2_PLACEMENT_3D('',#1000,#803,#804);
#671=AXIS2_PLACEMENT_3D('',#1001,#805,#806);
#672=AXIS2_PLACEMENT_3D('',#1003,#807,#808);
#673=AXIS2_PLACEMENT_3D('',#1004,#809,#810);
#674=AXIS2_PLACEMENT_3D('',#1006,#811,#812);
#675=AXIS2_PLACEMENT_3D('',#1007,#813,#814);
#676=AXIS2_PLACEMENT_3D('',#1008,#815,#816);
#677=AXIS2_PLACEMENT_3D('',#1011,#818,#819);
#678=AXIS2_PLACEMENT_3D('',#1012,#820,#821);
#679=AXIS2_PLACEMENT_3D('',#1014,#822,#823);
#680=AXIS2_PLACEMENT_3D('',#1015,#824,#825);
#681=AXIS2_PLACEMENT_3D('',#1016,#826,#827);
#682=AXIS2_PLACEMENT_3D('',#1017,#828,#829);
#683=AXIS2_PLACEMENT_3D('',#1018,#830,#831);
#684=AXIS2_PLACEMENT_3D('',#1020,#832,#833);
#685=AXIS2_PLACEMENT_3D('',#1021,#834,#835);
#686=AXIS2_PLACEMENT_3D('',#1023,#836,#837);
#687=AXIS2_PLACEMENT_3D('',#1024,#838,#839);
#688=AXIS2_PLACEMENT_3D('',#1026,#841,#842);
#689=AXIS2_PLACEMENT_3D('',#1027,#843,#844);
#690=AXIS2_PLACEMENT_3D('',#1029,#845,#846);
#691=AXIS2_PLACEMENT_3D('',#1030,#847,#848);
#692=AXIS2_PLACEMENT_3D('',#1032,#849,#850);
#693=AXIS2_PLACEMENT_3D('',#1033,#851,#852);
#694=AXIS2_PLACEMENT_3D('',#1035,#854,#855);
#695=AXIS2_PLACEMENT_3D('',#1036,#856,#857);
#696=AXIS2_PLACEMENT_3D('',#1038,#858,#859);
#697=AXIS2_PLACEMENT_3D('',#1041,#861,#862);
#698=AXIS2_PLACEMENT_3D('',#1042,#863,#864);
#699=AXIS2_PLACEMENT_3D('',#1044,#865,#866);
#700=AXIS2_PLACEMENT_3D('',#1046,#868,#869);
#701=AXIS2_PLACEMENT_3D('',#1049,#871,#872);
#702=AXIS2_PLACEMENT_3D('',#1050,#873,#874);
#703=AXIS2_PLACEMENT_3D('',#1051,#875,#876);
#704=AXIS2_PLACEMENT_3D('',#1052,#877,#878);
#705=AXIS2_PLACEMENT_3D('',#1053,#879,#880);
#706=AXIS2_PLACEMENT_3D('',#1055,#881,#882);
#707=AXIS2_PLACEMENT_3D('',#1056,#883,#884);
#708=AXIS2_PLACEMENT_3D('',#1058,#885,#886);
#709=AXIS2_PLACEMENT_3D('',#1059,#887,#888);
#710=AXIS2_PLACEMENT_3D('',#1061,#889,#890);
#711=AXIS2_PLACEMENT_3D('',#1062,#891,#892);
#712=AXIS2_PLACEMENT_3D('',#1063,#893,#894);
#713=AXIS2_PLACEMENT_3D('',#1065,#896,#897);
#714=AXIS2_PLACEMENT_3D('',#1066,#898,#899);
#715=AXIS2_PLACEMENT_3D('',#1069,#900,#901);
#716=AXIS2_PLACEMENT_3D('',#1072,#903,#904);
#717=AXIS2_PLACEMENT_3D('',#1073,#905,#906);
#718=AXIS2_PLACEMENT_3D('',#1074,#907,#908);
#719=AXIS2_PLACEMENT_3D('',#1078,#910,#911);
#720=AXIS2_PLACEMENT_3D('',#1079,#912,#913);
#721=AXIS2_PLACEMENT_3D('',#1080,#914,#915);
#722=AXIS2_PLACEMENT_3D('',#1081,#916,#917);
#723=AXIS2_PLACEMENT_3D('',#1084,#919,#920);
#724=AXIS2_PLACEMENT_3D('',#1085,#921,#922);
#725=AXIS2_PLACEMENT_3D('',#1086,#923,#924);
#726=AXIS2_PLACEMENT_3D('',#1087,#925,#926);
#727=AXIS2_PLACEMENT_3D('',#1089,#927,#928);
#728=AXIS2_PLACEMENT_3D('',#1090,#929,#930);
#729=AXIS2_PLACEMENT_3D('',#1092,#931,#932);
#730=AXIS2_PLACEMENT_3D('',#1093,#933,#934);
#731=AXIS2_PLACEMENT_3D('',#1095,#936,#937);
#732=AXIS2_PLACEMENT_3D('',#1096,#938,#939);
#733=AXIS2_PLACEMENT_3D('',#1097,#940,#941);
#734=AXIS2_PLACEMENT_3D('',#1098,#942,#943);
#735=AXIS2_PLACEMENT_3D('',#1099,#944,#945);
#736=AXIS2_PLACEMENT_3D('',#1100,#946,#947);
#737=AXIS2_PLACEMENT_3D('',#1101,#948,#949);
#738=AXIS2_PLACEMENT_3D('',#1102,#950,#951);
#739=AXIS2_PLACEMENT_3D('',#1103,#952,#953);
#740=AXIS2_PLACEMENT_3D('',#1104,#954,#955);
#741=DIRECTION('axis',(0.,0.,1.));
#742=DIRECTION('refdir',(1.,0.,0.));
#743=DIRECTION('axis',(0.,0.,1.));
#744=DIRECTION('refdir',(1.,0.,0.));
#745=DIRECTION('center_axis',(-1.,0.,0.));
#746=DIRECTION('ref_axis',(0.,0.,1.));
#747=DIRECTION('center_axis',(1.,0.,0.));
#748=DIRECTION('ref_axis',(0.,0.,-1.));
#749=DIRECTION('center_axis',(1.,0.,0.));
#750=DIRECTION('ref_axis',(0.,0.,-1.));
#751=DIRECTION('center_axis',(1.,0.,0.));
#752=DIRECTION('ref_axis',(0.,0.,-1.));
#753=DIRECTION('',(-1.,0.,0.));
#754=DIRECTION('center_axis',(1.,0.,0.));
#755=DIRECTION('ref_axis',(0.,0.,-1.));
#756=DIRECTION('axis',(0.,0.,1.));
#757=DIRECTION('refdir',(1.,0.,0.));
#758=DIRECTION('center_axis',(1.,0.,0.));
#759=DIRECTION('ref_axis',(0.,0.,-1.));
#760=DIRECTION('center_axis',(1.,0.,0.));
#761=DIRECTION('ref_axis',(0.,0.,-1.));
#762=DIRECTION('',(-0.975408410378343,2.69918469288288E-17,-0.220405156389757));
#763=DIRECTION('center_axis',(1.,0.,0.));
#764=DIRECTION('ref_axis',(0.,0.,-1.));
#765=DIRECTION('center_axis',(1.,0.,0.));
#766=DIRECTION('ref_axis',(0.,0.,-1.));
#767=DIRECTION('center_axis',(1.,0.,0.));
#768=DIRECTION('ref_axis',(0.,0.,-1.));
#769=DIRECTION('',(-1.,0.,0.));
#770=DIRECTION('center_axis',(1.,0.,0.));
#771=DIRECTION('ref_axis',(0.,0.,-1.));
#772=DIRECTION('center_axis',(1.,0.,0.));
#773=DIRECTION('ref_axis',(0.,0.,-1.));
#774=DIRECTION('',(-0.828718159042203,6.85393373868948E-17,-0.559666161987396));
#775=DIRECTION('center_axis',(1.,0.,0.));
#776=DIRECTION('ref_axis',(0.,0.,-1.));
#777=DIRECTION('center_axis',(1.,0.,0.));
#778=DIRECTION('ref_axis',(0.,0.,-1.));
#779=DIRECTION('',(-1.,0.,0.));
#780=DIRECTION('center_axis',(1.,0.,0.));
#781=DIRECTION('ref_axis',(0.,0.,-1.));
#782=DIRECTION('center_axis',(1.,0.,0.));
#783=DIRECTION('ref_axis',(0.,0.,-1.));
#784=DIRECTION('center_axis',(0.,-1.,-1.22464679914735E-16));
#785=DIRECTION('ref_axis',(0.,-1.22464679914735E-16,1.));
#786=DIRECTION('center_axis',(1.,0.,0.));
#787=DIRECTION('ref_axis',(0.,0.,-1.));
#788=DIRECTION('center_axis',(-1.,0.,0.));
#789=DIRECTION('ref_axis',(0.,0.,1.));
#790=DIRECTION('axis',(0.,0.,1.));
#791=DIRECTION('refdir',(1.,0.,0.));
#792=DIRECTION('center_axis',(1.,0.,0.));
#793=DIRECTION('ref_axis',(0.,0.,-1.));
#794=DIRECTION('center_axis',(1.,0.,0.));
#795=DIRECTION('ref_axis',(0.,0.,-1.));
#796=DIRECTION('',(-1.,0.,0.));
#797=DIRECTION('center_axis',(1.,0.,0.));
#798=DIRECTION('ref_axis',(0.,0.,-1.));
#799=DIRECTION('center_axis',(1.,0.,0.));
#800=DIRECTION('ref_axis',(0.,0.,-1.));
#801=DIRECTION('center_axis',(-1.,0.,0.));
#802=DIRECTION('ref_axis',(0.,0.,1.));
#803=DIRECTION('axis',(0.,0.,1.));
#804=DIRECTION('refdir',(1.,0.,0.));
#805=DIRECTION('center_axis',(-1.,0.,0.));
#806=DIRECTION('ref_axis',(0.,0.,1.));
#807=DIRECTION('center_axis',(1.,0.,0.));
#808=DIRECTION('ref_axis',(0.,0.,-1.));
#809=DIRECTION('center_axis',(1.,0.,0.));
#810=DIRECTION('ref_axis',(0.,0.,-1.));
#811=DIRECTION('center_axis',(1.,0.,0.));
#812=DIRECTION('ref_axis',(0.,0.,-1.));
#813=DIRECTION('center_axis',(0.,-1.,-1.22464679914735E-16));
#814=DIRECTION('ref_axis',(0.,-1.22464679914735E-16,1.));
#815=DIRECTION('center_axis',(-1.,0.,0.));
#816=DIRECTION('ref_axis',(0.,0.,-1.));
#817=DIRECTION('',(0.998209609000375,-7.32496099175571E-18,-0.0598128456045909));
#818=DIRECTION('center_axis',(1.,0.,0.));
#819=DIRECTION('ref_axis',(0.,0.,-1.));
#820=DIRECTION('center_axis',(1.,0.,0.));
#821=DIRECTION('ref_axis',(0.,0.,-1.));
#822=DIRECTION('center_axis',(1.,0.,0.));
#823=DIRECTION('ref_axis',(0.,0.,-1.));
#824=DIRECTION('center_axis',(0.,-1.,-1.22464679914735E-16));
#825=DIRECTION('ref_axis',(0.,-1.22464679914735E-16,1.));
#826=DIRECTION('center_axis',(1.,0.,0.));
#827=DIRECTION('ref_axis',(0.,0.,-1.));
#828=DIRECTION('axis',(0.,0.,1.));
#829=DIRECTION('refdir',(1.,0.,0.));
#830=DIRECTION('center_axis',(1.,0.,0.));
#831=DIRECTION('ref_axis',(0.,0.,-1.));
#832=DIRECTION('center_axis',(1.,0.,0.));
#833=DIRECTION('ref_axis',(0.,0.,-1.));
#834=DIRECTION('center_axis',(-1.,0.,0.));
#835=DIRECTION('ref_axis',(0.,0.,1.));
#836=DIRECTION('center_axis',(1.,0.,0.));
#837=DIRECTION('ref_axis',(0.,0.,-1.));
#838=DIRECTION('center_axis',(1.,0.,0.));
#839=DIRECTION('ref_axis',(0.,0.,-1.));
#840=DIRECTION('',(-1.,0.,0.));
#841=DIRECTION('axis',(0.,0.,1.));
#842=DIRECTION('refdir',(1.,0.,0.));
#843=DIRECTION('center_axis',(1.,0.,0.));
#844=DIRECTION('ref_axis',(0.,0.,-1.));
#845=DIRECTION('center_axis',(1.,0.,0.));
#846=DIRECTION('ref_axis',(0.,0.,-1.));
#847=DIRECTION('center_axis',(-1.,0.,0.));
#848=DIRECTION('ref_axis',(0.,0.,1.));
#849=DIRECTION('center_axis',(1.,0.,0.));
#850=DIRECTION('ref_axis',(0.,0.,-1.));
#851=DIRECTION('center_axis',(1.,0.,0.));
#852=DIRECTION('ref_axis',(0.,0.,-1.));
#853=DIRECTION('',(-1.,0.,0.));
#854=DIRECTION('axis',(0.,0.,1.));
#855=DIRECTION('refdir',(1.,0.,0.));
#856=DIRECTION('center_axis',(1.,0.,0.));
#857=DIRECTION('ref_axis',(0.,0.,-1.));
#858=DIRECTION('center_axis',(1.,0.,0.));
#859=DIRECTION('ref_axis',(0.,0.,-1.));
#860=DIRECTION('',(-0.707106781186546,8.65956056235496E-17,-0.707106781186549));
#861=DIRECTION('center_axis',(1.,0.,0.));
#862=DIRECTION('ref_axis',(0.,0.,-1.));
#863=DIRECTION('center_axis',(1.,0.,0.));
#864=DIRECTION('ref_axis',(0.,0.,-1.));
#865=DIRECTION('center_axis',(1.,0.,0.));
#866=DIRECTION('ref_axis',(0.,0.,-1.));
#867=DIRECTION('',(-1.,0.,0.));
#868=DIRECTION('center_axis',(-1.,0.,0.));
#869=DIRECTION('ref_axis',(0.,0.,-1.));
#870=DIRECTION('',(0.707106781186546,-8.65956056235496E-17,-0.707106781186549));
#871=DIRECTION('center_axis',(1.,0.,0.));
#872=DIRECTION('ref_axis',(0.,0.,-1.));
#873=DIRECTION('center_axis',(1.,0.,0.));
#874=DIRECTION('ref_axis',(0.,0.,-1.));
#875=DIRECTION('center_axis',(-1.,0.,0.));
#876=DIRECTION('ref_axis',(0.,0.,1.));
#877=DIRECTION('axis',(0.,0.,1.));
#878=DIRECTION('refdir',(1.,0.,0.));
#879=DIRECTION('center_axis',(1.,0.,0.));
#880=DIRECTION('ref_axis',(0.,0.,-1.));
#881=DIRECTION('center_axis',(1.,0.,0.));
#882=DIRECTION('ref_axis',(0.,0.,-1.));
#883=DIRECTION('center_axis',(-1.,0.,0.));
#884=DIRECTION('ref_axis',(0.,0.,1.));
#885=DIRECTION('center_axis',(1.,0.,0.));
#886=DIRECTION('ref_axis',(0.,0.,-1.));
#887=DIRECTION('center_axis',(1.,0.,0.));
#888=DIRECTION('ref_axis',(0.,0.,-1.));
#889=DIRECTION('center_axis',(1.,0.,0.));
#890=DIRECTION('ref_axis',(0.,0.,-1.));
#891=DIRECTION('center_axis',(0.,-1.,-1.22464679914735E-16));
#892=DIRECTION('ref_axis',(0.,-1.22464679914735E-16,1.));
#893=DIRECTION('center_axis',(1.,0.,0.));
#894=DIRECTION('ref_axis',(0.,0.,-1.));
#895=DIRECTION('',(-1.,0.,0.));
#896=DIRECTION('axis',(0.,0.,1.));
#897=DIRECTION('refdir',(1.,0.,0.));
#898=DIRECTION('center_axis',(-1.,0.,0.));
#899=DIRECTION('ref_axis',(0.,0.,1.));
#900=DIRECTION('center_axis',(1.,0.,0.));
#901=DIRECTION('ref_axis',(0.,0.,1.));
#902=DIRECTION('',(0.70710678118655,8.6595605623549E-17,0.707106781186545));
#903=DIRECTION('center_axis',(-1.,0.,0.));
#904=DIRECTION('ref_axis',(0.,0.,1.));
#905=DIRECTION('center_axis',(1.,0.,0.));
#906=DIRECTION('ref_axis',(0.,0.,1.));
#907=DIRECTION('center_axis',(1.,0.,0.));
#908=DIRECTION('ref_axis',(0.,0.,-1.));
#909=DIRECTION('',(-1.,0.,0.));
#910=DIRECTION('center_axis',(-1.,0.,0.));
#911=DIRECTION('ref_axis',(0.,0.,1.));
#912=DIRECTION('center_axis',(-1.,0.,0.));
#913=DIRECTION('ref_axis',(0.,0.,1.));
#914=DIRECTION('center_axis',(1.,0.,0.));
#915=DIRECTION('ref_axis',(0.,0.,-1.));
#916=DIRECTION('center_axis',(1.,0.,0.));
#917=DIRECTION('ref_axis',(0.,0.,1.));
#918=DIRECTION('',(-0.707106781186545,-8.65956056235497E-17,0.70710678118655));
#919=DIRECTION('center_axis',(1.,0.,0.));
#920=DIRECTION('ref_axis',(0.,0.,1.));
#921=DIRECTION('center_axis',(-1.,0.,0.));
#922=DIRECTION('ref_axis',(0.,0.,1.));
#923=DIRECTION('axis',(0.,0.,1.));
#924=DIRECTION('refdir',(1.,0.,0.));
#925=DIRECTION('center_axis',(1.,0.,0.));
#926=DIRECTION('ref_axis',(0.,0.,-1.));
#927=DIRECTION('center_axis',(1.,0.,0.));
#928=DIRECTION('ref_axis',(0.,0.,-1.));
#929=DIRECTION('center_axis',(-1.,0.,0.));
#930=DIRECTION('ref_axis',(0.,0.,1.));
#931=DIRECTION('center_axis',(1.,0.,0.));
#932=DIRECTION('ref_axis',(0.,0.,-1.));
#933=DIRECTION('center_axis',(1.,0.,0.));
#934=DIRECTION('ref_axis',(0.,0.,-1.));
#935=DIRECTION('',(-1.,0.,0.));
#936=DIRECTION('',(0.,0.,1.));
#937=DIRECTION('',(1.,0.,0.));
#938=DIRECTION('',(0.,0.,1.));
#939=DIRECTION('',(1.,0.,0.));
#940=DIRECTION('',(0.,0.,1.));
#941=DIRECTION('',(1.,0.,0.));
#942=DIRECTION('',(0.,0.,1.));
#943=DIRECTION('',(1.,0.,0.));
#944=DIRECTION('',(0.,0.,1.));
#945=DIRECTION('',(1.,0.,0.));
#946=DIRECTION('',(0.,0.,1.));
#947=DIRECTION('',(1.,0.,0.));
#948=DIRECTION('',(0.,0.,1.));
#949=DIRECTION('',(1.,0.,0.));
#950=DIRECTION('',(0.,0.,1.));
#951=DIRECTION('',(1.,0.,0.));
#952=DIRECTION('',(0.,0.,1.));
#953=DIRECTION('',(1.,0.,0.));
#954=DIRECTION('',(0.,0.,1.));
#955=DIRECTION('',(1.,0.,0.));
#956=CARTESIAN_POINT('',(0.,0.,0.));
#957=CARTESIAN_POINT('',(0.,0.,0.));
#958=CARTESIAN_POINT('Origin',(0.,0.,-3.));
#959=CARTESIAN_POINT('',(0.,-3.67394039744206E-16,3.));
#960=CARTESIAN_POINT('Origin',(0.,0.,0.));
#961=CARTESIAN_POINT('Origin',(9.11772158674436,0.,0.));
#962=CARTESIAN_POINT('',(18.2354431734887,-3.67394039744206E-16,3.));
#963=CARTESIAN_POINT('Origin',(18.2354431734887,0.,0.));
#964=CARTESIAN_POINT('',(9.11772158674436,-3.67394039744206E-16,3.));
#965=CARTESIAN_POINT('Origin',(18.2354431734887,0.,0.));
#966=CARTESIAN_POINT('',(0.,0.,0.));
#967=CARTESIAN_POINT('Origin',(49.7315453550068,0.,0.));
#968=CARTESIAN_POINT('',(52.1545159854134,-8.52857666836739E-16,6.96411134565927));
#969=CARTESIAN_POINT('Origin',(52.1545159854134,0.,0.));
#970=CARTESIAN_POINT('',(47.3085747246001,-7.18759064296257E-16,5.86911315815046));
#971=CARTESIAN_POINT('',(49.7315453550068,-7.85808365566499E-16,6.41661225190487));
#972=CARTESIAN_POINT('Origin',(47.3085747246001,0.,0.));
#973=CARTESIAN_POINT('Origin',(59.8855873271505,0.,0.));
#974=CARTESIAN_POINT('',(67.6166586688876,-8.52857666836739E-16,6.96411134565927));
#975=CARTESIAN_POINT('Origin',(67.6166586688876,0.,0.));
#976=CARTESIAN_POINT('',(59.8855873271505,-8.52857666836739E-16,6.96411134565927));
#977=CARTESIAN_POINT('Origin',(67.8860694496847,0.,0.));
#978=CARTESIAN_POINT('',(68.1554802304818,-8.97421035454263E-16,7.327998865298));
#979=CARTESIAN_POINT('Origin',(68.1554802304818,0.,0.));
#980=CARTESIAN_POINT('',(67.8860694496847,-8.75139351145501E-16,7.14605510547863));
#981=CARTESIAN_POINT('Origin',(76.6276350483148,0.,0.));
#982=CARTESIAN_POINT('',(85.0997898661478,-8.97421035454263E-16,7.327998865298));
#983=CARTESIAN_POINT('Origin',(85.0997898661478,0.,0.));
#984=CARTESIAN_POINT('',(76.6276350483148,-8.97421035454263E-16,7.327998865298));
#985=CARTESIAN_POINT('Origin',(85.0997898661478,0.,0.));
#986=CARTESIAN_POINT('',(86.5997898661478,-7.1372401558216E-16,5.827998865298));
#987=CARTESIAN_POINT('Origin',(86.5997898661478,0.,0.));
#988=CARTESIAN_POINT('Origin',(85.0997898661478,-7.13724015582159E-16,5.82799886529799));
#989=CARTESIAN_POINT('Origin',(86.5997898661478,0.,0.));
#990=CARTESIAN_POINT('Origin',(47.3085747246001,0.,-5.86911315815046));
#991=CARTESIAN_POINT('',(0.,0.,0.));
#992=CARTESIAN_POINT('Origin',(87.7281259529897,0.,0.));
#993=CARTESIAN_POINT('',(88.8564620398316,-3.93169537221952E-16,3.21047290937838));
#994=CARTESIAN_POINT('Origin',(88.8564620398316,0.,0.));
#995=CARTESIAN_POINT('',(86.5997898661478,-3.93169537221952E-16,3.21047290937838));
#996=CARTESIAN_POINT('',(87.7281259529897,-3.93169537221952E-16,3.21047290937838));
#997=CARTESIAN_POINT('Origin',(86.5997898661478,0.,0.));
#998=CARTESIAN_POINT('Origin',(88.8564620398316,0.,0.));
#999=CARTESIAN_POINT('Origin',(86.5997898661478,0.,-3.21047290937838));
#1000=CARTESIAN_POINT('',(0.,0.,0.));
#1001=CARTESIAN_POINT('Origin',(88.8564620398316,0.,-3.3075988470339));
#1002=CARTESIAN_POINT('',(88.8564620398316,-4.05064034088354E-16,3.3075988470339));
#1003=CARTESIAN_POINT('Origin',(88.8564620398316,0.,0.));
#1004=CARTESIAN_POINT('Origin',(89.3564620398316,0.,0.));
#1005=CARTESIAN_POINT('',(89.3863684626339,-4.66186744215375E-16,3.80670365153407));
#1006=CARTESIAN_POINT('Origin',(89.3863684626339,0.,0.));
#1007=CARTESIAN_POINT('Origin',(89.3564620398316,-4.05064034088354E-16,
3.3075988470339));
#1008=CARTESIAN_POINT('Origin',(94.4581374427181,0.,0.));
#1009=CARTESIAN_POINT('',(99.5299064228023,-3.91752457862398E-16,3.1989015782767));
#1010=CARTESIAN_POINT('',(94.4581374427181,4.28969601038887E-16,3.50280261490539));
#1011=CARTESIAN_POINT('Origin',(99.5299064228023,0.,0.));
#1012=CARTESIAN_POINT('Origin',(99.5,0.,0.));
#1013=CARTESIAN_POINT('',(100.,-3.30629747735376E-16,2.69979677377651));
#1014=CARTESIAN_POINT('Origin',(100.,0.,0.));
#1015=CARTESIAN_POINT('Origin',(99.5,-3.30629747735373E-16,2.69979677377649));
#1016=CARTESIAN_POINT('Origin',(100.,0.,0.));
#1017=CARTESIAN_POINT('',(0.,0.,0.));
#1018=CARTESIAN_POINT('Origin',(31.0379185953459,0.,0.));
#1019=CARTESIAN_POINT('',(31.0379185953459,-4.89858719658941E-16,4.));
#1020=CARTESIAN_POINT('Origin',(31.0379185953459,0.,0.));
#1021=CARTESIAN_POINT('Origin',(23.2354431734887,0.,-4.));
#1022=CARTESIAN_POINT('',(23.2354431734887,-4.89858719658941E-16,4.));
#1023=CARTESIAN_POINT('Origin',(23.2354431734887,0.,0.));
#1024=CARTESIAN_POINT('Origin',(27.1366808844173,0.,0.));
#1025=CARTESIAN_POINT('',(27.1366808844173,-4.89858719658941E-16,4.));
#1026=CARTESIAN_POINT('',(0.,0.,0.));
#1027=CARTESIAN_POINT('Origin',(20.2354431734887,0.,0.));
#1028=CARTESIAN_POINT('',(20.2354431734887,-4.89858719658941E-16,4.));
#1029=CARTESIAN_POINT('Origin',(20.2354431734887,0.,0.));
#1030=CARTESIAN_POINT('Origin',(18.2354431734887,0.,-4.));
#1031=CARTESIAN_POINT('',(18.2354431734887,-4.89858719658941E-16,4.));
#1032=CARTESIAN_POINT('Origin',(18.2354431734887,0.,0.));
#1033=CARTESIAN_POINT('Origin',(19.2354431734887,0.,0.));
#1034=CARTESIAN_POINT('',(19.2354431734887,-4.89858719658941E-16,4.));
#1035=CARTESIAN_POINT('',(0.,0.,0.));
#1036=CARTESIAN_POINT('Origin',(20.4854431734887,0.,0.));
#1037=CARTESIAN_POINT('',(20.7354431734887,-7.34788079488412E-16,6.));
#1038=CARTESIAN_POINT('Origin',(20.7354431734887,0.,0.));
#1039=CARTESIAN_POINT('',(20.2354431734887,-6.73555739531044E-16,5.5));
#1040=CARTESIAN_POINT('',(20.4854431734887,-7.04171909509728E-16,5.75));
#1041=CARTESIAN_POINT('Origin',(20.2354431734887,0.,0.));
#1042=CARTESIAN_POINT('Origin',(21.7354431734887,0.,0.));
#1043=CARTESIAN_POINT('',(22.7354431734887,-7.34788079488412E-16,6.));
#1044=CARTESIAN_POINT('Origin',(22.7354431734887,0.,0.));
#1045=CARTESIAN_POINT('',(21.7354431734887,-7.34788079488412E-16,6.));
#1046=CARTESIAN_POINT('Origin',(22.9854431734887,0.,0.));
#1047=CARTESIAN_POINT('',(23.2354431734887,-6.73555739531044E-16,5.5));
#1048=CARTESIAN_POINT('',(22.9854431734887,7.04171909509728E-16,5.75));
#1049=CARTESIAN_POINT('Origin',(23.2354431734887,0.,0.));
#1050=CARTESIAN_POINT('Origin',(23.2354431734887,0.,0.));
#1051=CARTESIAN_POINT('Origin',(20.2354431734887,0.,-5.5));
#1052=CARTESIAN_POINT('',(0.,0.,0.));
#1053=CARTESIAN_POINT('Origin',(31.9264360344922,0.,0.));
#1054=CARTESIAN_POINT('',(31.9264360344922,-8.16757743755127E-16,6.66933310342039));
#1055=CARTESIAN_POINT('Origin',(31.9264360344922,0.,0.));
#1056=CARTESIAN_POINT('Origin',(31.0379185953459,0.,-6.16933310342039));
#1057=CARTESIAN_POINT('',(31.0379185953459,-7.55525403797759E-16,6.16933310342039));
#1058=CARTESIAN_POINT('Origin',(31.0379185953459,0.,0.));
#1059=CARTESIAN_POINT('Origin',(31.5379185953459,0.,0.));
#1060=CARTESIAN_POINT('',(31.5379185953459,-8.16757743755127E-16,6.66933310342039));
#1061=CARTESIAN_POINT('Origin',(31.5379185953459,0.,0.));
#1062=CARTESIAN_POINT('Origin',(31.5379185953459,-7.5552540379776E-16,6.1693331034204));
#1063=CARTESIAN_POINT('Origin',(31.7321773149191,0.,0.));
#1064=CARTESIAN_POINT('',(31.7321773149191,-8.16757743755127E-16,6.66933310342039));
#1065=CARTESIAN_POINT('',(0.,0.,0.));
#1066=CARTESIAN_POINT('Origin',(40.2408939752243,0.,0.));
#1067=CARTESIAN_POINT('',(40.0908939752243,-9.5706132001803E-16,7.81499874644978));
#1068=CARTESIAN_POINT('',(40.0908939752243,-9.5706132001803E-16,-7.81499874644978));
#1069=CARTESIAN_POINT('Origin',(40.0908939752243,0.,0.));
#1070=CARTESIAN_POINT('',(40.3908939752244,-9.2032191604361E-16,-7.51499874644978));
#1071=CARTESIAN_POINT('',(40.2408939752243,-9.3869161803082E-16,-7.66499874644978));
#1072=CARTESIAN_POINT('Origin',(40.3908939752244,0.,0.));
#1073=CARTESIAN_POINT('Origin',(40.0908939752243,0.,0.));
#1074=CARTESIAN_POINT('Origin',(36.1586650048583,0.,0.));
#1075=CARTESIAN_POINT('',(32.2264360344922,-9.5706132001803E-16,7.81499874644978));
#1076=CARTESIAN_POINT('',(36.1586650048583,-9.5706132001803E-16,7.81499874644978));
#1077=CARTESIAN_POINT('',(32.2264360344922,-9.5706132001803E-16,-7.81499874644978));
#1078=CARTESIAN_POINT('Origin',(32.2264360344922,0.,0.));
#1079=CARTESIAN_POINT('Origin',(32.2264360344922,0.,0.));
#1080=CARTESIAN_POINT('Origin',(40.3908939752244,0.,0.));
#1081=CARTESIAN_POINT('Origin',(32.0764360344922,0.,0.));
#1082=CARTESIAN_POINT('',(31.9264360344922,9.2032191604361E-16,-7.51499874644978));
#1083=CARTESIAN_POINT('',(32.0764360344922,9.3869161803082E-16,-7.66499874644978));
#1084=CARTESIAN_POINT('Origin',(31.9264360344922,0.,0.));
#1085=CARTESIAN_POINT('Origin',(31.9264360344922,0.,-7.81499874644978));
#1086=CARTESIAN_POINT('',(0.,0.,0.));
#1087=CARTESIAN_POINT('Origin',(47.3085747246001,0.,0.));
#1088=CARTESIAN_POINT('',(47.3085747246001,-6.71421499357961E-16,5.48257260644808));
#1089=CARTESIAN_POINT('Origin',(47.3085747246001,0.,0.));
#1090=CARTESIAN_POINT('Origin',(40.3908939752244,0.,-5.48257260644808));
#1091=CARTESIAN_POINT('',(40.3908939752244,-6.71421499357961E-16,5.48257260644808));
#1092=CARTESIAN_POINT('Origin',(40.3908939752244,0.,0.));
#1093=CARTESIAN_POINT('Origin',(43.8497343499122,0.,0.));
#1094=CARTESIAN_POINT('',(43.8497343499122,-6.7142149935796E-16,5.48257260644808));
#1095=CARTESIAN_POINT('',(0.,0.,0.));
#1096=CARTESIAN_POINT('',(0.,0.,0.));
#1097=CARTESIAN_POINT('',(0.,0.,0.));
#1098=CARTESIAN_POINT('',(0.,0.,0.));
#1099=CARTESIAN_POINT('',(0.,0.,0.));
#1100=CARTESIAN_POINT('',(0.,0.,0.));
#1101=CARTESIAN_POINT('',(0.,0.,0.));
#1102=CARTESIAN_POINT('',(0.,0.,0.));
#1103=CARTESIAN_POINT('',(0.,0.,0.));
#1104=CARTESIAN_POINT('',(0.,0.,0.));
#1105=UNCERTAINTY_MEASURE_WITH_UNIT(LENGTH_MEASURE(0.01),#1129,
'DISTANCE_ACCURACY_VALUE',
'Maximum model space distance between geometric entities at asserted c
onnectivities');
#1106=UNCERTAINTY_MEASURE_WITH_UNIT(LENGTH_MEASURE(0.01),#1129,
'DISTANCE_ACCURACY_VALUE',
'Maximum model space distance between geometric entities at asserted c
onnectivities');
#1107=UNCERTAINTY_MEASURE_WITH_UNIT(LENGTH_MEASURE(0.01),#1129,
'DISTANCE_ACCURACY_VALUE',
'Maximum model space distance between geometric entities at asserted c
onnectivities');
#1108=UNCERTAINTY_MEASURE_WITH_UNIT(LENGTH_MEASURE(0.01),#1129,
'DISTANCE_ACCURACY_VALUE',
'Maximum model space distance between geometric entities at asserted c
onnectivities');
#1109=UNCERTAINTY_MEASURE_WITH_UNIT(LENGTH_MEASURE(0.01),#1129,
'DISTANCE_ACCURACY_VALUE',
'Maximum model space distance between geometric entities at asserted c
onnectivities');
#1110=UNCERTAINTY_MEASURE_WITH_UNIT(LENGTH_MEASURE(0.01),#1129,
'DISTANCE_ACCURACY_VALUE',
'Maximum model space distance between geometric entities at asserted c
onnectivities');
#1111=UNCERTAINTY_MEASURE_WITH_UNIT(LENGTH_MEASURE(0.01),#1129,
'DISTANCE_ACCURACY_VALUE',
'Maximum model space distance between geometric entities at asserted c
onnectivities');
#1112=UNCERTAINTY_MEASURE_WITH_UNIT(LENGTH_MEASURE(0.01),#1129,
'DISTANCE_ACCURACY_VALUE',
'Maximum model space distance between geometric entities at asserted c
onnectivities');
#1113=UNCERTAINTY_MEASURE_WITH_UNIT(LENGTH_MEASURE(0.01),#1129,
'DISTANCE_ACCURACY_VALUE',
'Maximum model space distance between geometric entities at asserted c
onnectivities');
#1114=UNCERTAINTY_MEASURE_WITH_UNIT(LENGTH_MEASURE(0.01),#1129,
'DISTANCE_ACCURACY_VALUE',
'Maximum model space distance between geometric entities at asserted c
onnectivities');
#1115=UNCERTAINTY_MEASURE_WITH_UNIT(LENGTH_MEASURE(0.01),#1129,
'DISTANCE_ACCURACY_VALUE',
'Maximum model space distance between geometric entities at asserted c
onnectivities');
#1116=UNCERTAINTY_MEASURE_WITH_UNIT(LENGTH_MEASURE(0.01),#1129,
'DISTANCE_ACCURACY_VALUE',
'Maximum model space distance between geometric entities at asserted c
onnectivities');
#1117=(
GEOMETRIC_REPRESENTATION_CONTEXT(3)
GLOBAL_UNCERTAINTY_ASSIGNED_CONTEXT((#1105))
GLOBAL_UNIT_ASSIGNED_CONTEXT((#1129,#1131,#1132))
REPRESENTATION_CONTEXT('','3D')
);
#1118=(
GEOMETRIC_REPRESENTATION_CONTEXT(3)
GLOBAL_UNCERTAINTY_ASSIGNED_CONTEXT((#1106))
GLOBAL_UNIT_ASSIGNED_CONTEXT((#1129,#1131,#1132))
REPRESENTATION_CONTEXT('','3D')
);
#1119=(
GEOMETRIC_REPRESENTATION_CONTEXT(3)
GLOBAL_UNCERTAINTY_ASSIGNED_CONTEXT((#1107))
GLOBAL_UNIT_ASSIGNED_CONTEXT((#1129,#1131,#1132))
REPRESENTATION_CONTEXT('','3D')
);
#1120=(
GEOMETRIC_REPRESENTATION_CONTEXT(3)
GLOBAL_UNCERTAINTY_ASSIGNED_CONTEXT((#1108))
GLOBAL_UNIT_ASSIGNED_CONTEXT((#1129,#1131,#1132))
REPRESENTATION_CONTEXT('','3D')
);
#1121=(
GEOMETRIC_REPRESENTATION_CONTEXT(3)
GLOBAL_UNCERTAINTY_ASSIGNED_CONTEXT((#1109))
GLOBAL_UNIT_ASSIGNED_CONTEXT((#1129,#1131,#1132))
REPRESENTATION_CONTEXT('','3D')
);
#1122=(
GEOMETRIC_REPRESENTATION_CONTEXT(3)
GLOBAL_UNCERTAINTY_ASSIGNED_CONTEXT((#1110))
GLOBAL_UNIT_ASSIGNED_CONTEXT((#1129,#1131,#1132))
REPRESENTATION_CONTEXT('','3D')
);
#1123=(
GEOMETRIC_REPRESENTATION_CONTEXT(3)
GLOBAL_UNCERTAINTY_ASSIGNED_CONTEXT((#1111))
GLOBAL_UNIT_ASSIGNED_CONTEXT((#1129,#1131,#1132))
REPRESENTATION_CONTEXT('','3D')
);
#1124=(
GEOMETRIC_REPRESENTATION_CONTEXT(3)
GLOBAL_UNCERTAINTY_ASSIGNED_CONTEXT((#1112))
GLOBAL_UNIT_ASSIGNED_CONTEXT((#1129,#1131,#1132))
REPRESENTATION_CONTEXT('','3D')
);
#1125=(
GEOMETRIC_REPRESENTATION_CONTEXT(3)
GLOBAL_UNCERTAINTY_ASSIGNED_CONTEXT((#1113))
GLOBAL_UNIT_ASSIGNED_CONTEXT((#1129,#1131,#1132))
REPRESENTATION_CONTEXT('','3D')
);
#1126=(
GEOMETRIC_REPRESENTATION_CONTEXT(3)
GLOBAL_UNCERTAINTY_ASSIGNED_CONTEXT((#1114))
GLOBAL_UNIT_ASSIGNED_CONTEXT((#1129,#1131,#1132))
REPRESENTATION_CONTEXT('','3D')
);
#1127=(
GEOMETRIC_REPRESENTATION_CONTEXT(3)
GLOBAL_UNCERTAINTY_ASSIGNED_CONTEXT((#1115))
GLOBAL_UNIT_ASSIGNED_CONTEXT((#1129,#1131,#1132))
REPRESENTATION_CONTEXT('','3D')
);
#1128=(
GEOMETRIC_REPRESENTATION_CONTEXT(3)
GLOBAL_UNCERTAINTY_ASSIGNED_CONTEXT((#1116))
GLOBAL_UNIT_ASSIGNED_CONTEXT((#1129,#1131,#1132))
REPRESENTATION_CONTEXT('','3D')
);
#1129=(
LENGTH_UNIT()
NAMED_UNIT(*)
SI_UNIT(.MILLI.,.METRE.)
);
#1130=(
LENGTH_UNIT()
NAMED_UNIT(*)
SI_UNIT($,.METRE.)
);
#1131=(
NAMED_UNIT(*)
PLANE_ANGLE_UNIT()
SI_UNIT($,.RADIAN.)
);
#1132=(
NAMED_UNIT(*)
SI_UNIT($,.STERADIAN.)
SOLID_ANGLE_UNIT()
);
#1133=SHAPE_DEFINITION_REPRESENTATION(#1144,#1165);
#1134=SHAPE_DEFINITION_REPRESENTATION(#1145,#1166);
#1135=SHAPE_DEFINITION_REPRESENTATION(#1146,#1167);
#1136=SHAPE_DEFINITION_REPRESENTATION(#1147,#1168);
#1137=SHAPE_DEFINITION_REPRESENTATION(#1148,#1169);
#1138=SHAPE_DEFINITION_REPRESENTATION(#1149,#1170);
#1139=SHAPE_DEFINITION_REPRESENTATION(#1150,#1171);
#1140=SHAPE_DEFINITION_REPRESENTATION(#1151,#1172);
#1141=SHAPE_DEFINITION_REPRESENTATION(#1152,#1173);
#1142=SHAPE_DEFINITION_REPRESENTATION(#1153,#1174);
#1143=SHAPE_DEFINITION_REPRESENTATION(#1154,#1175);
#1144=PRODUCT_DEFINITION_SHAPE('',$,#1177);
#1145=PRODUCT_DEFINITION_SHAPE('',$,#1178);
#1146=PRODUCT_DEFINITION_SHAPE('',$,#1179);
#1147=PRODUCT_DEFINITION_SHAPE('',$,#1180);
#1148=PRODUCT_DEFINITION_SHAPE('',$,#1181);
#1149=PRODUCT_DEFINITION_SHAPE('',$,#1182);
#1150=PRODUCT_DEFINITION_SHAPE('',$,#1183);
#1151=PRODUCT_DEFINITION_SHAPE('',$,#1184);
#1152=PRODUCT_DEFINITION_SHAPE('',$,#1185);
#1153=PRODUCT_DEFINITION_SHAPE('',$,#1186);
#1154=PRODUCT_DEFINITION_SHAPE('',$,#1187);
#1155=PRODUCT_DEFINITION_SHAPE($,$,#41);
#1156=PRODUCT_DEFINITION_SHAPE($,$,#42);
#1157=PRODUCT_DEFINITION_SHAPE($,$,#43);
#1158=PRODUCT_DEFINITION_SHAPE($,$,#44);
#1159=PRODUCT_DEFINITION_SHAPE($,$,#45);
#1160=PRODUCT_DEFINITION_SHAPE($,$,#46);
#1161=PRODUCT_DEFINITION_SHAPE($,$,#47);
#1162=PRODUCT_DEFINITION_SHAPE($,$,#48);
#1163=PRODUCT_DEFINITION_SHAPE($,$,#49);
#1164=PRODUCT_DEFINITION_SHAPE($,$,#50);
#1165=SHAPE_REPRESENTATION('',(#642,#731,#732,#733,#734,#735,#736,#737,
#738,#739,#740),#1117);
#1166=SHAPE_REPRESENTATION('',(#643),#1118);
#1167=SHAPE_REPRESENTATION('',(#649),#1119);
#1168=SHAPE_REPRESENTATION('',(#664),#1120);
#1169=SHAPE_REPRESENTATION('',(#670),#1121);
#1170=SHAPE_REPRESENTATION('',(#682),#1122);
#1171=SHAPE_REPRESENTATION('',(#688),#1123);
#1172=SHAPE_REPRESENTATION('',(#694),#1124);
#1173=SHAPE_REPRESENTATION('',(#704),#1125);
#1174=SHAPE_REPRESENTATION('',(#713),#1126);
#1175=SHAPE_REPRESENTATION('',(#725),#1127);
#1176=PRODUCT_DEFINITION_CONTEXT('part definition',#1211,'design');
#1177=PRODUCT_DEFINITION('BR-156','BR-156',#1188,#1176);
#1178=PRODUCT_DEFINITION('Rod','Rod',#1189,#1176);
#1179=PRODUCT_DEFINITION('Thimble','Thimble',#1190,#1176);
#1180=PRODUCT_DEFINITION('Lock_Ring_02','Lock_Ring_02',#1191,#1176);
#1181=PRODUCT_DEFINITION('Knob','Knob',#1192,#1176);
#1182=PRODUCT_DEFINITION('Flange','Flange',#1193,#1176);
#1183=PRODUCT_DEFINITION('Ring','Ring',#1194,#1176);
#1184=PRODUCT_DEFINITION('Nut','Nut',#1195,#1176);
#1185=PRODUCT_DEFINITION('Sleeve','Sleeve',#1196,#1176);
#1186=PRODUCT_DEFINITION('Lock_Ring','Lock_Ring',#1197,#1176);
#1187=PRODUCT_DEFINITION('Collar','Collar',#1198,#1176);
#1188=PRODUCT_DEFINITION_FORMATION('',$,#1213);
#1189=PRODUCT_DEFINITION_FORMATION('',$,#1214);
#1190=PRODUCT_DEFINITION_FORMATION('',$,#1215);
#1191=PRODUCT_DEFINITION_FORMATION('',$,#1216);
#1192=PRODUCT_DEFINITION_FORMATION('',$,#1217);
#1193=PRODUCT_DEFINITION_FORMATION('',$,#1218);
#1194=PRODUCT_DEFINITION_FORMATION('',$,#1219);
#1195=PRODUCT_DEFINITION_FORMATION('',$,#1220);
#1196=PRODUCT_DEFINITION_FORMATION('',$,#1221);
#1197=PRODUCT_DEFINITION_FORMATION('',$,#1222);
#1198=PRODUCT_DEFINITION_FORMATION('',$,#1223);
#1199=PRODUCT_RELATED_PRODUCT_CATEGORY('BR-156','BR-156',(#1213));
#1200=PRODUCT_RELATED_PRODUCT_CATEGORY('Rod','Rod',(#1214));
#1201=PRODUCT_RELATED_PRODUCT_CATEGORY('Thimble','Thimble',(#1215));
#1202=PRODUCT_RELATED_PRODUCT_CATEGORY('Lock_Ring_02','Lock_Ring_02',(#1216));
#1203=PRODUCT_RELATED_PRODUCT_CATEGORY('Knob','Knob',(#1217));
#1204=PRODUCT_RELATED_PRODUCT_CATEGORY('Flange','Flange',(#1218));
#1205=PRODUCT_RELATED_PRODUCT_CATEGORY('Ring','Ring',(#1219));
#1206=PRODUCT_RELATED_PRODUCT_CATEGORY('Nut','Nut',(#1220));
#1207=PRODUCT_RELATED_PRODUCT_CATEGORY('Sleeve','Sleeve',(#1221));
#1208=PRODUCT_RELATED_PRODUCT_CATEGORY('Lock_Ring','Lock_Ring',(#1222));
#1209=PRODUCT_RELATED_PRODUCT_CATEGORY('Collar','Collar',(#1223));
#1210=APPLICATION_PROTOCOL_DEFINITION('international standard',
'automotive_design',2009,#1211);
#1211=APPLICATION_CONTEXT(
'Core Data for Automotive Mechanical Design Process');
#1212=PRODUCT_CONTEXT('part definition',#1211,'mechanical');
#1213=PRODUCT('BR-156','BR-156',$,(#1212));
#1214=PRODUCT('Rod','Rod',$,(#1212));
#1215=PRODUCT('Thimble','Thimble',$,(#1212));
#1216=PRODUCT('Lock_Ring_02','Lock_Ring_02',$,(#1212));
#1217=PRODUCT('Knob','Knob',$,(#1212));
#1218=PRODUCT('Flange','Flange',$,(#1212));
#1219=PRODUCT('Ring','Ring',$,(#1212));
#1220=PRODUCT('Nut','Nut',$,(#1212));
#1221=PRODUCT('Sleeve','Sleeve',$,(#1212));
#1222=PRODUCT('Lock_Ring','Lock_Ring',$,(#1212));
#1223=PRODUCT('Collar','Collar',$,(#1212));
#1224=PRESENTATION_STYLE_ASSIGNMENT((#1228));
#1225=PRESENTATION_STYLE_ASSIGNMENT((#1229));
#1226=PRESENTATION_STYLE_ASSIGNMENT((#1230));
#1227=PRESENTATION_STYLE_ASSIGNMENT((#1231));
#1228=SURFACE_STYLE_USAGE(.BOTH.,#1232);
#1229=SURFACE_STYLE_USAGE(.BOTH.,#1233);
#1230=SURFACE_STYLE_USAGE(.BOTH.,#1234);
#1231=SURFACE_STYLE_USAGE(.BOTH.,#1235);
#1232=SURFACE_SIDE_STYLE('',(#1236));
#1233=SURFACE_SIDE_STYLE('',(#1237));
#1234=SURFACE_SIDE_STYLE('',(#1238));
#1235=SURFACE_SIDE_STYLE('',(#1239));
#1236=SURFACE_STYLE_FILL_AREA(#1240);
#1237=SURFACE_STYLE_FILL_AREA(#1241);
#1238=SURFACE_STYLE_FILL_AREA(#1242);
#1239=SURFACE_STYLE_FILL_AREA(#1243);
#1240=FILL_AREA_STYLE('Steel - Satin',(#1244));
#1241=FILL_AREA_STYLE('Opaque(201,201,201)',(#1245));
#1242=FILL_AREA_STYLE('Opaque(94,95,15)',(#1246));
#1243=FILL_AREA_STYLE('Opaque(77,77,77)',(#1247));
#1244=FILL_AREA_STYLE_COLOUR('Steel - Satin',#1248);
#1245=FILL_AREA_STYLE_COLOUR('Opaque(201,201,201)',#1249);
#1246=FILL_AREA_STYLE_COLOUR('Opaque(94,95,15)',#1250);
#1247=FILL_AREA_STYLE_COLOUR('Opaque(77,77,77)',#1251);
#1248=COLOUR_RGB('Steel - Satin', 0.09019608, 0.27058824, 0.51372549);
#1249=COLOUR_RGB('Opaque(201,201,201)', 0.09019608, 0.27058824, 0.51372549);
#1250=COLOUR_RGB('Opaque(94,95,15)', 0.31764706, 0.68627451, 0.89019608);
#1251=COLOUR_RGB('Opaque(77,77,77)', 0.72549020, 0.75294118, 0.79215686);
ENDSEC;
END-ISO-10303-21;
